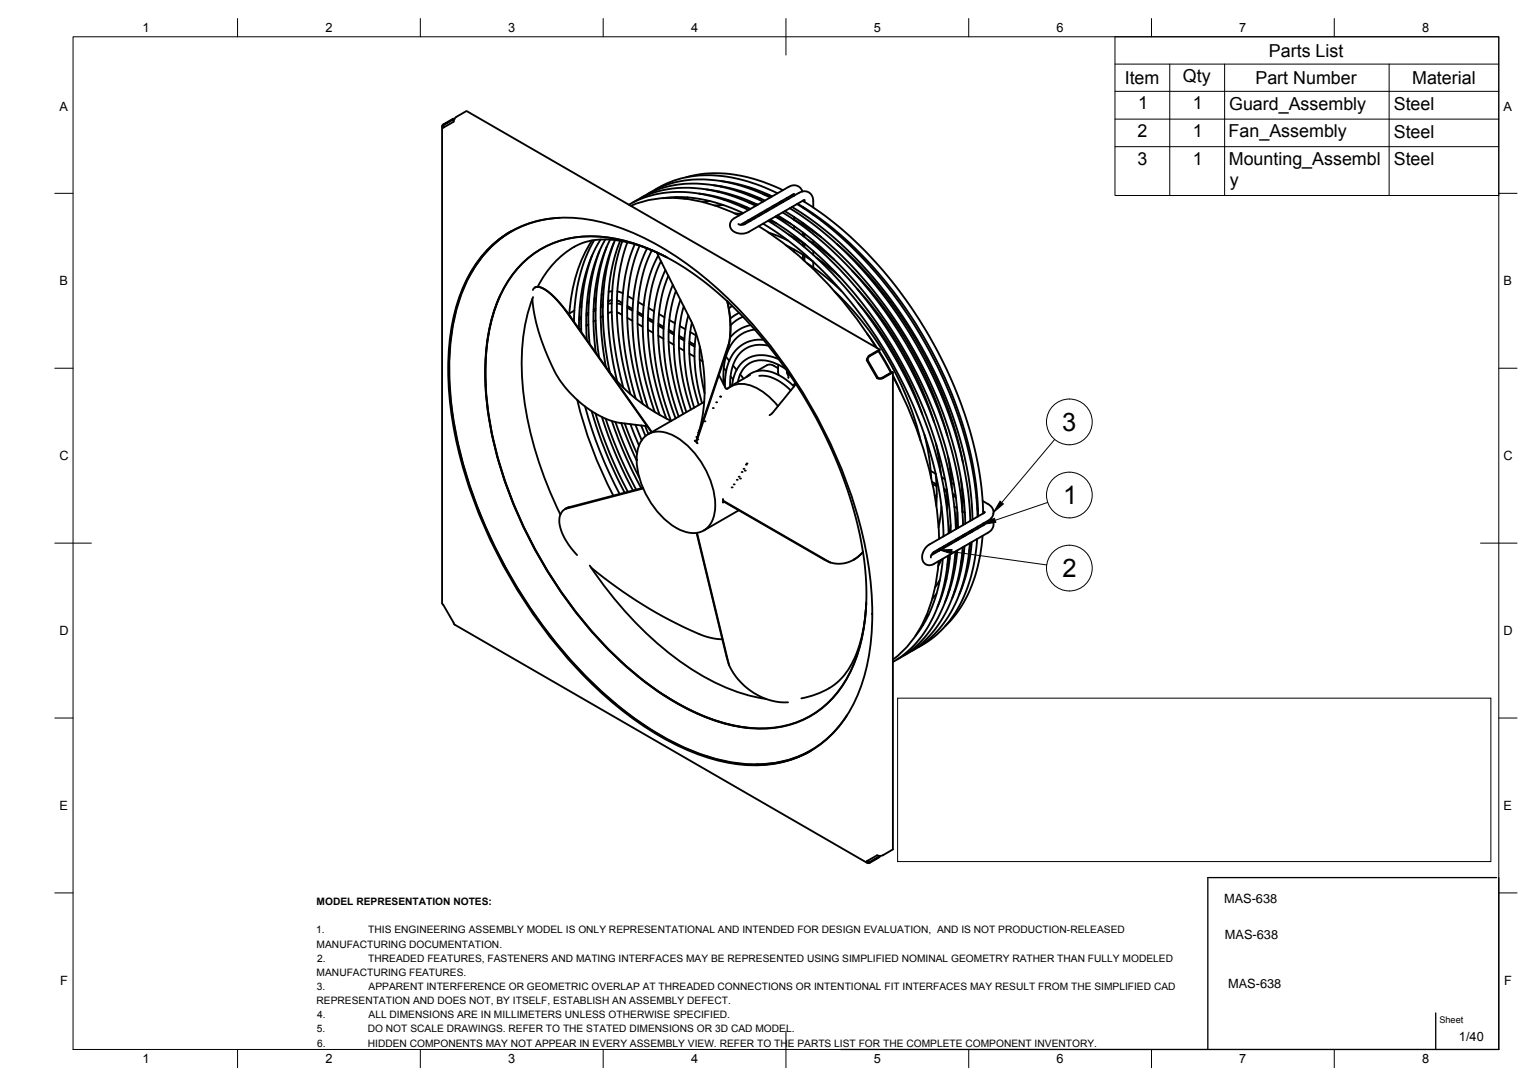
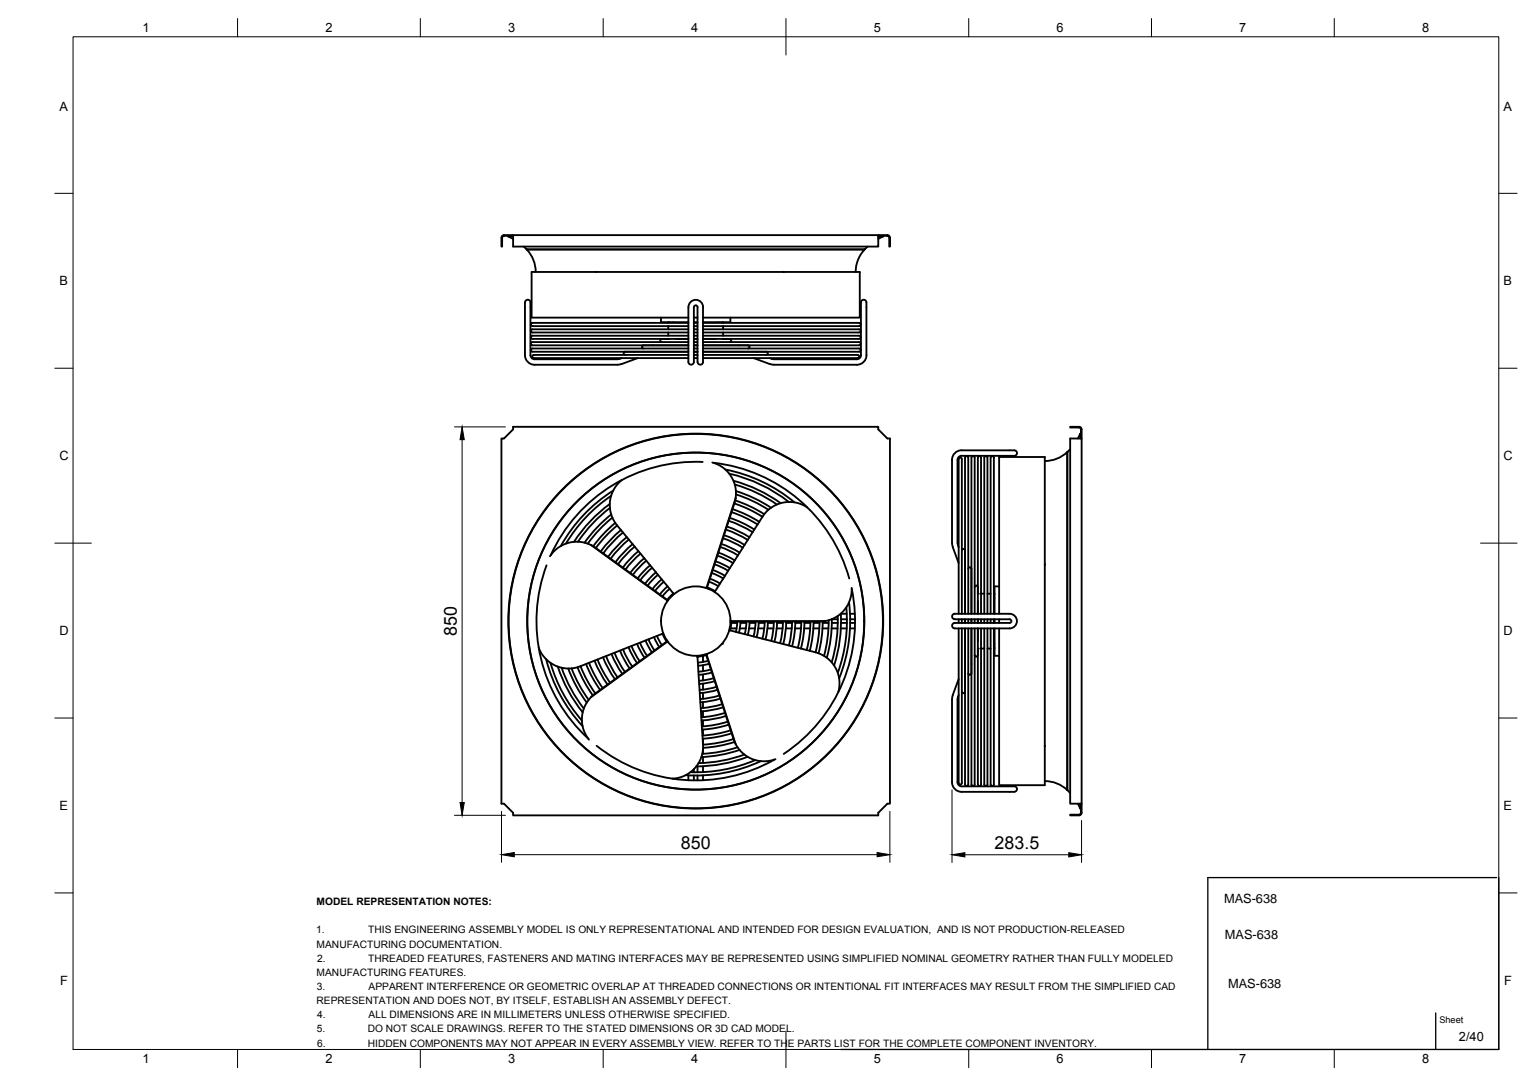
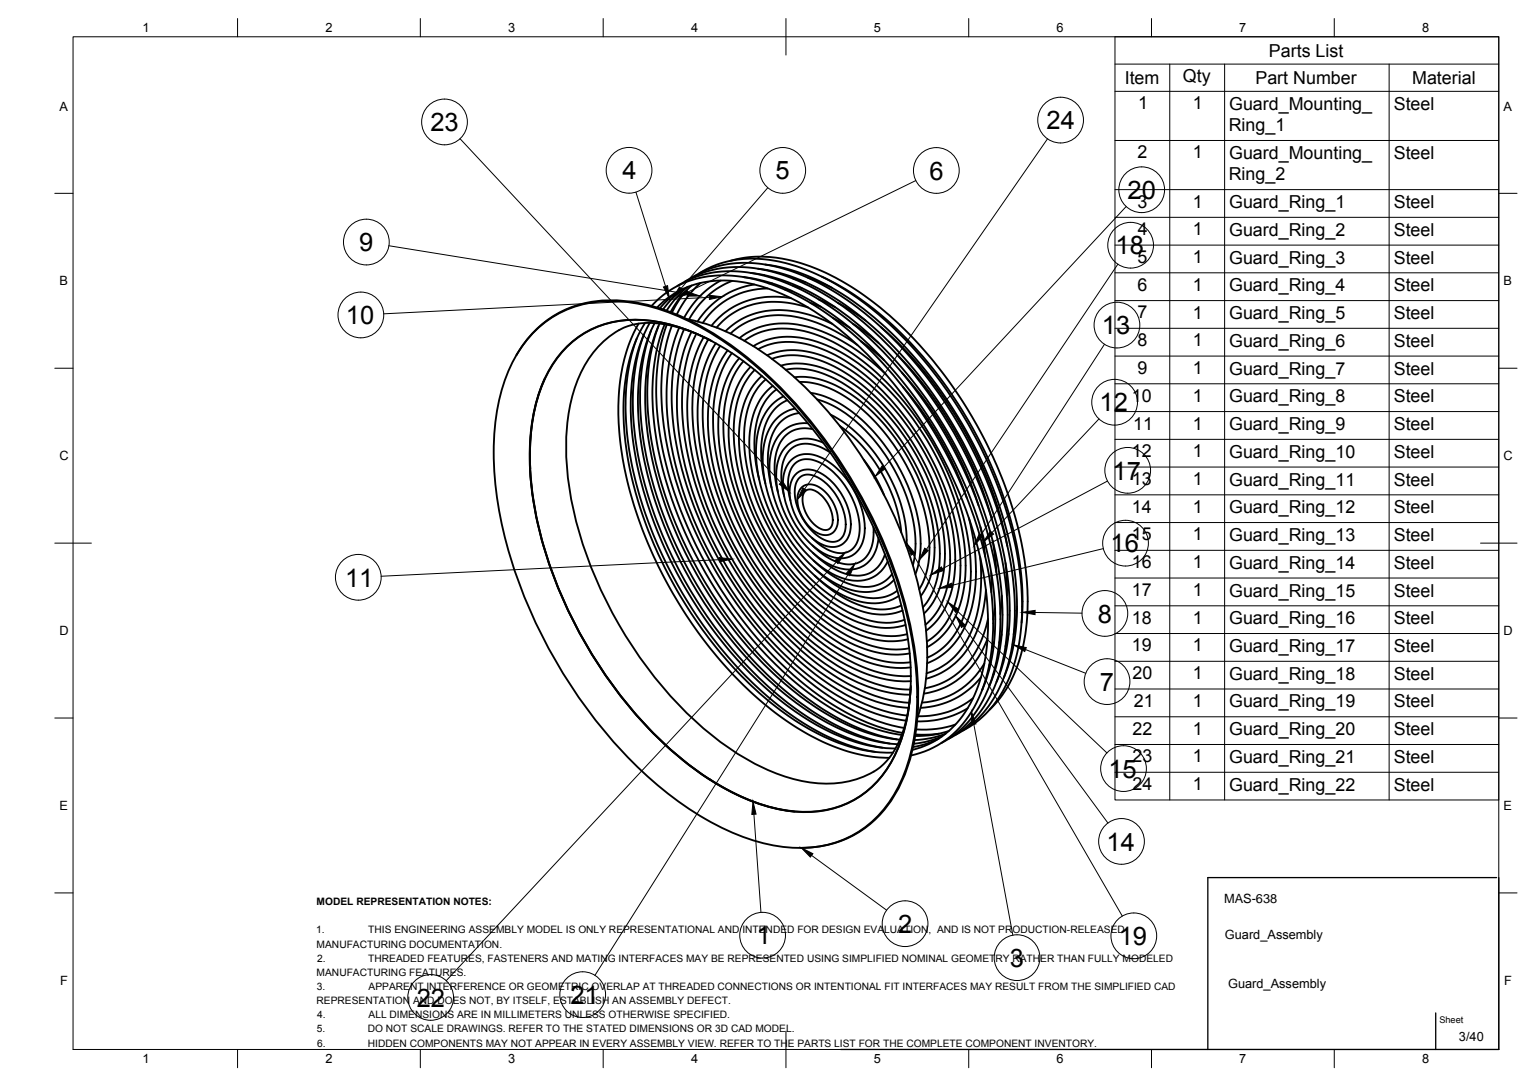
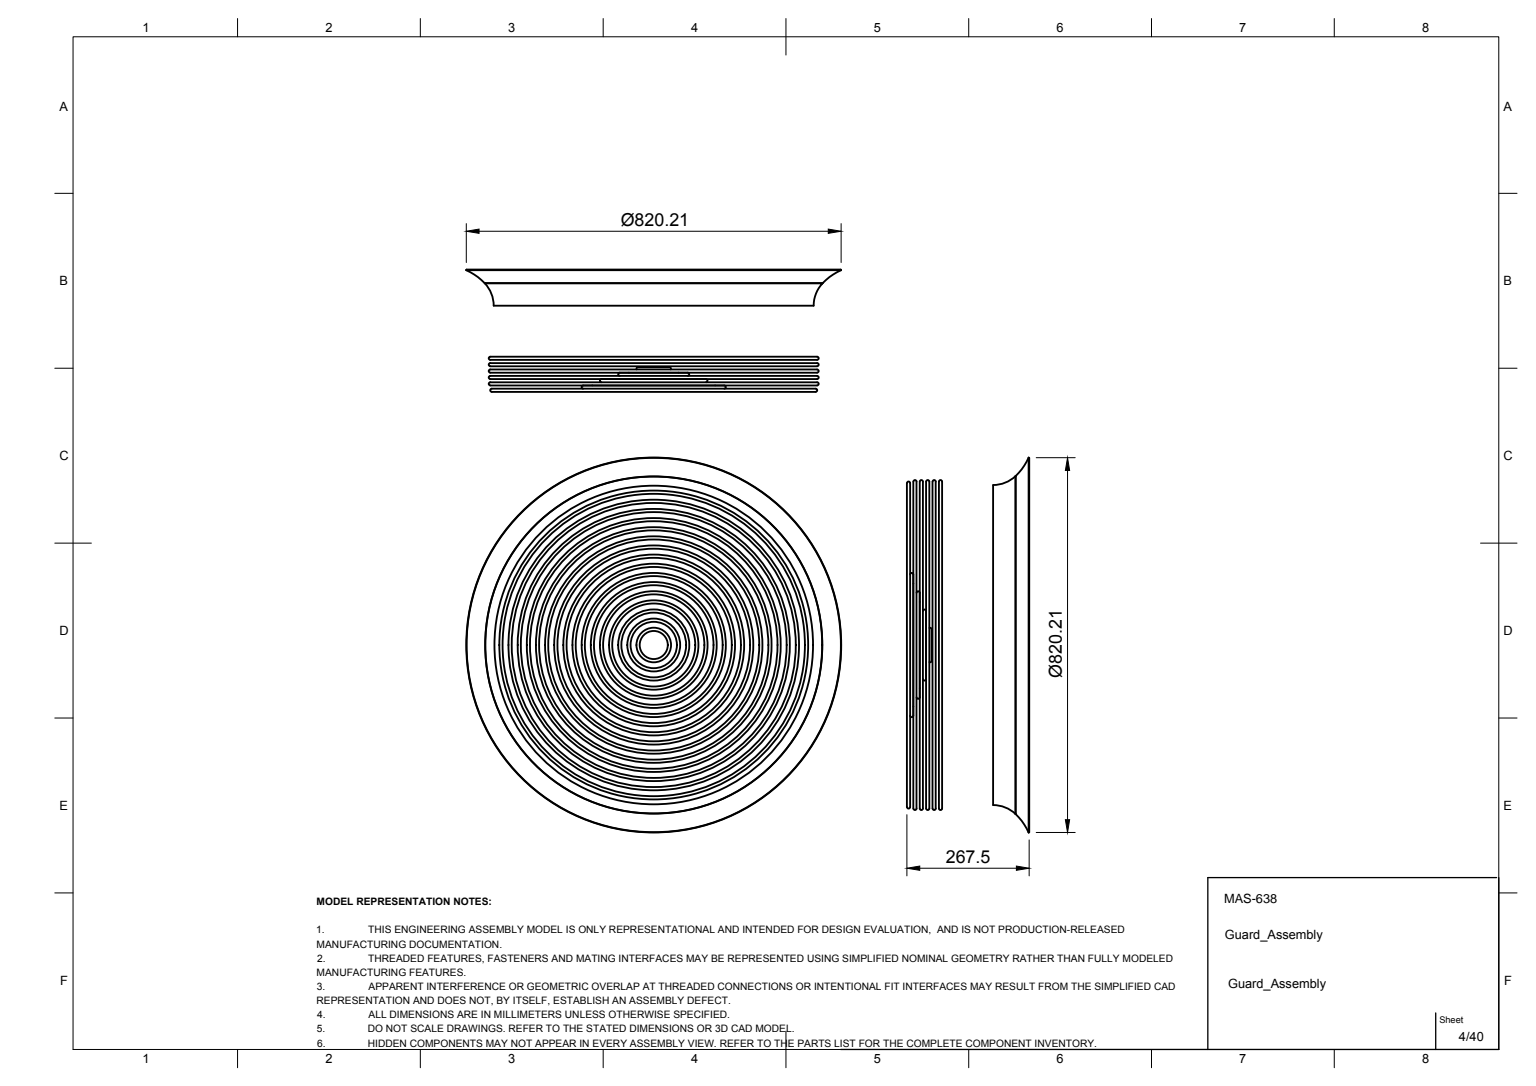
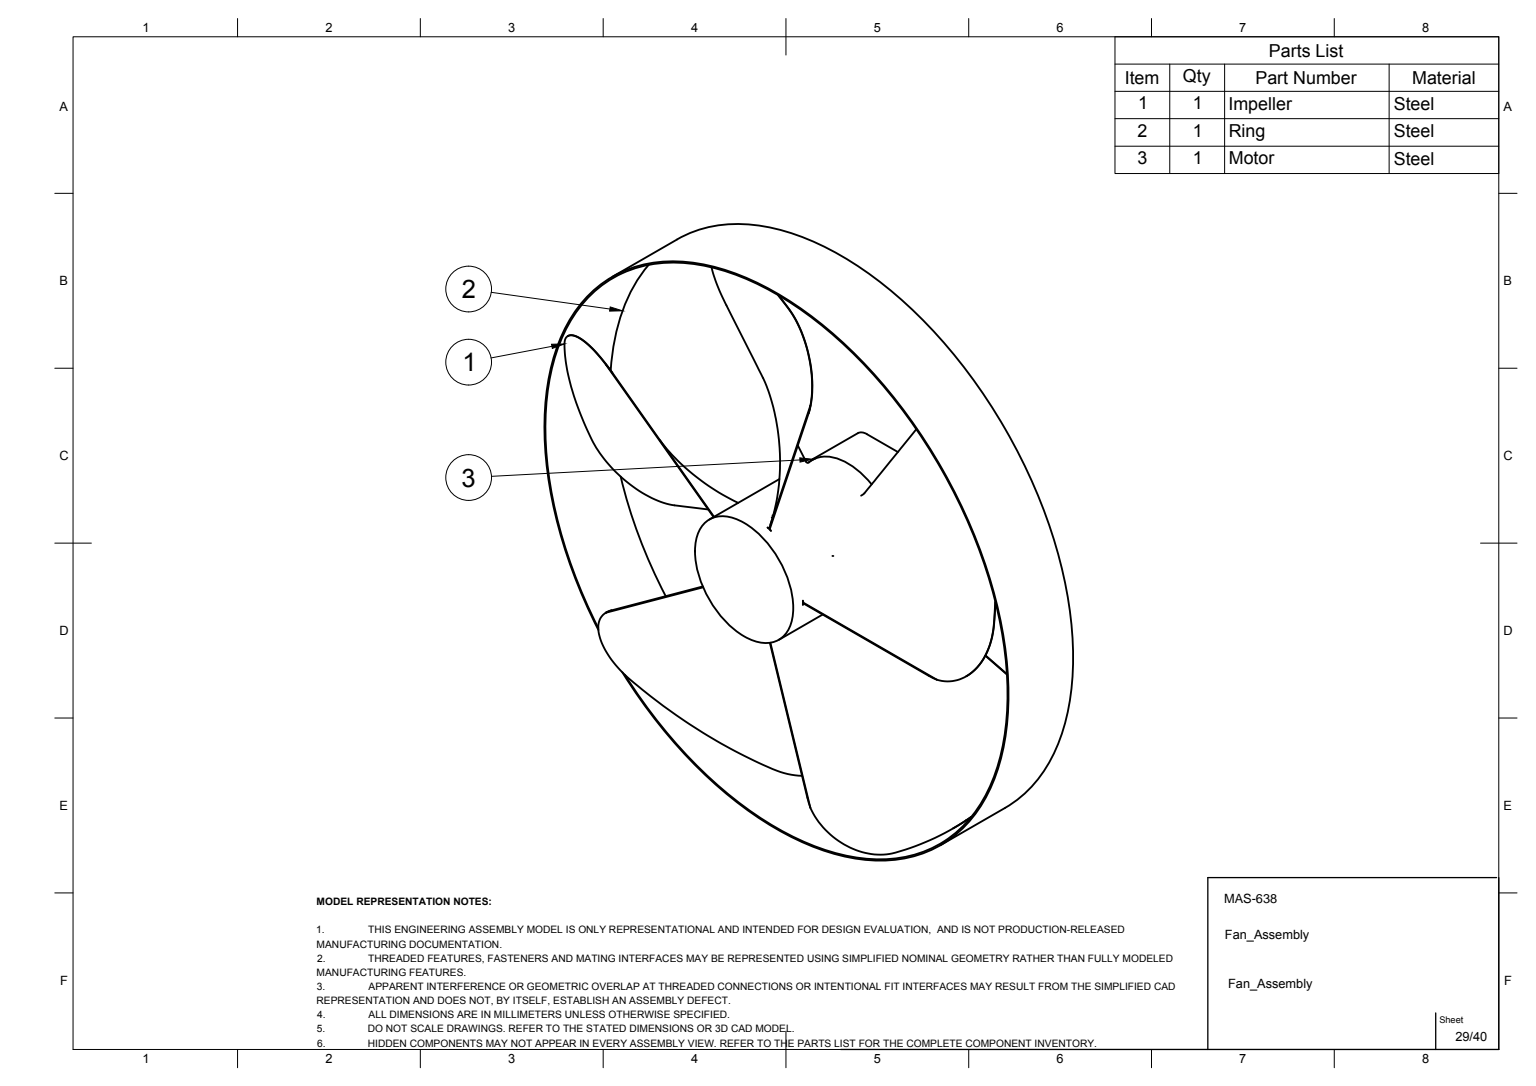
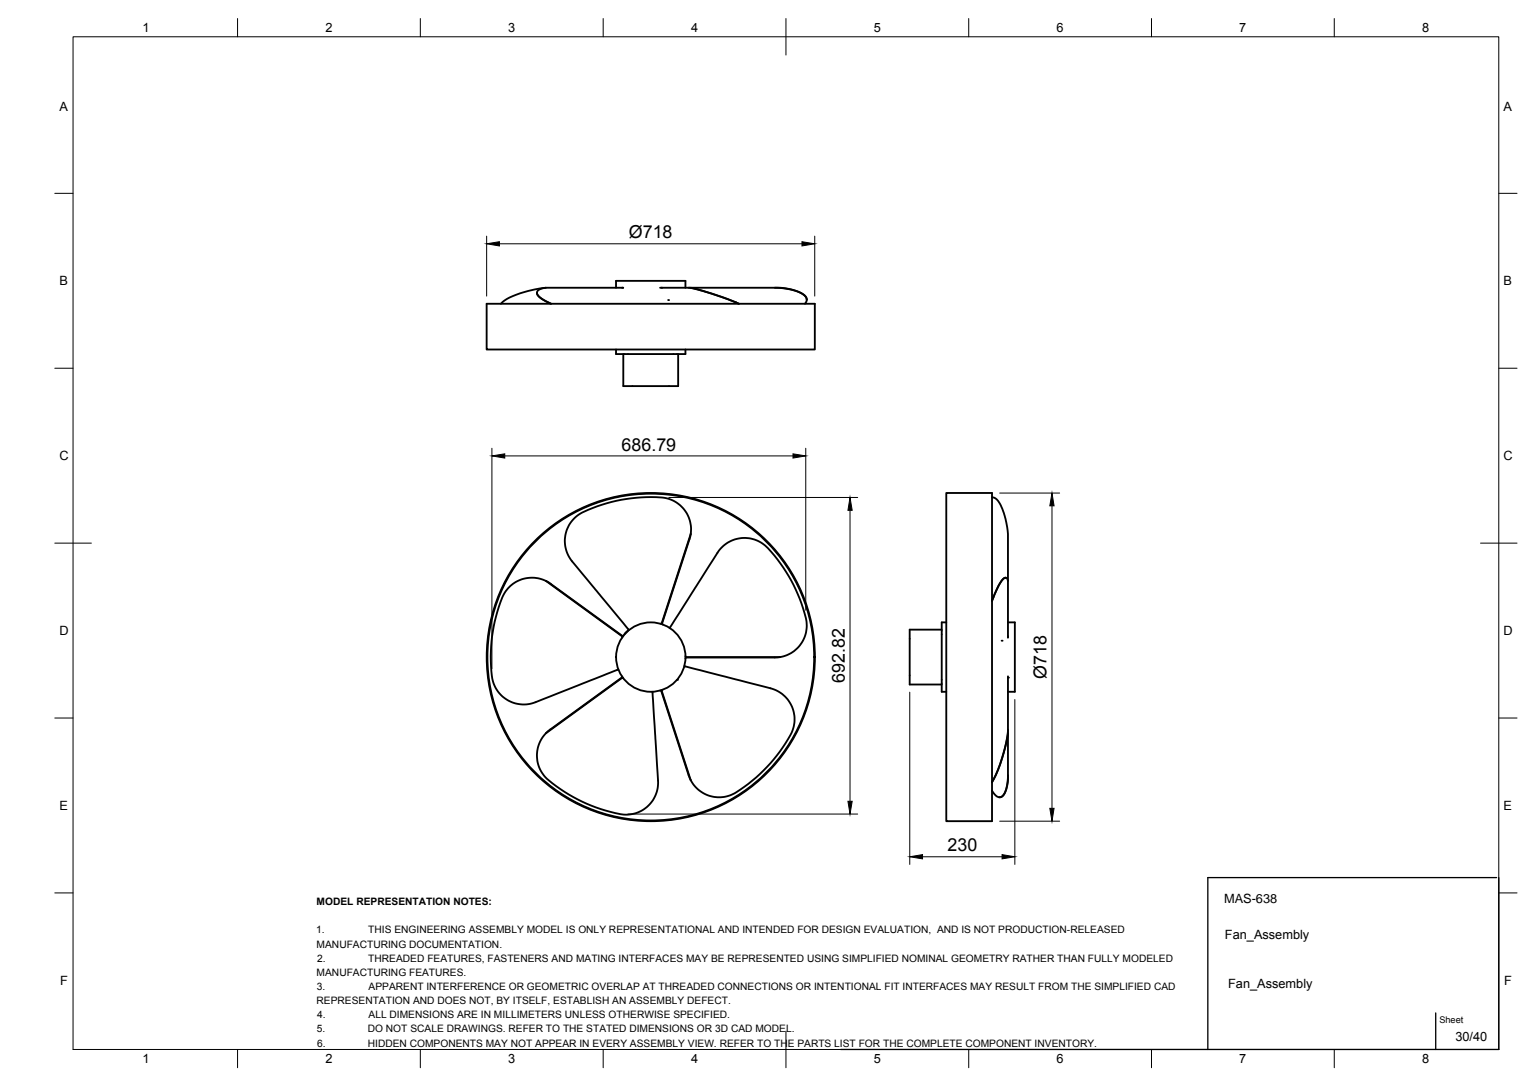
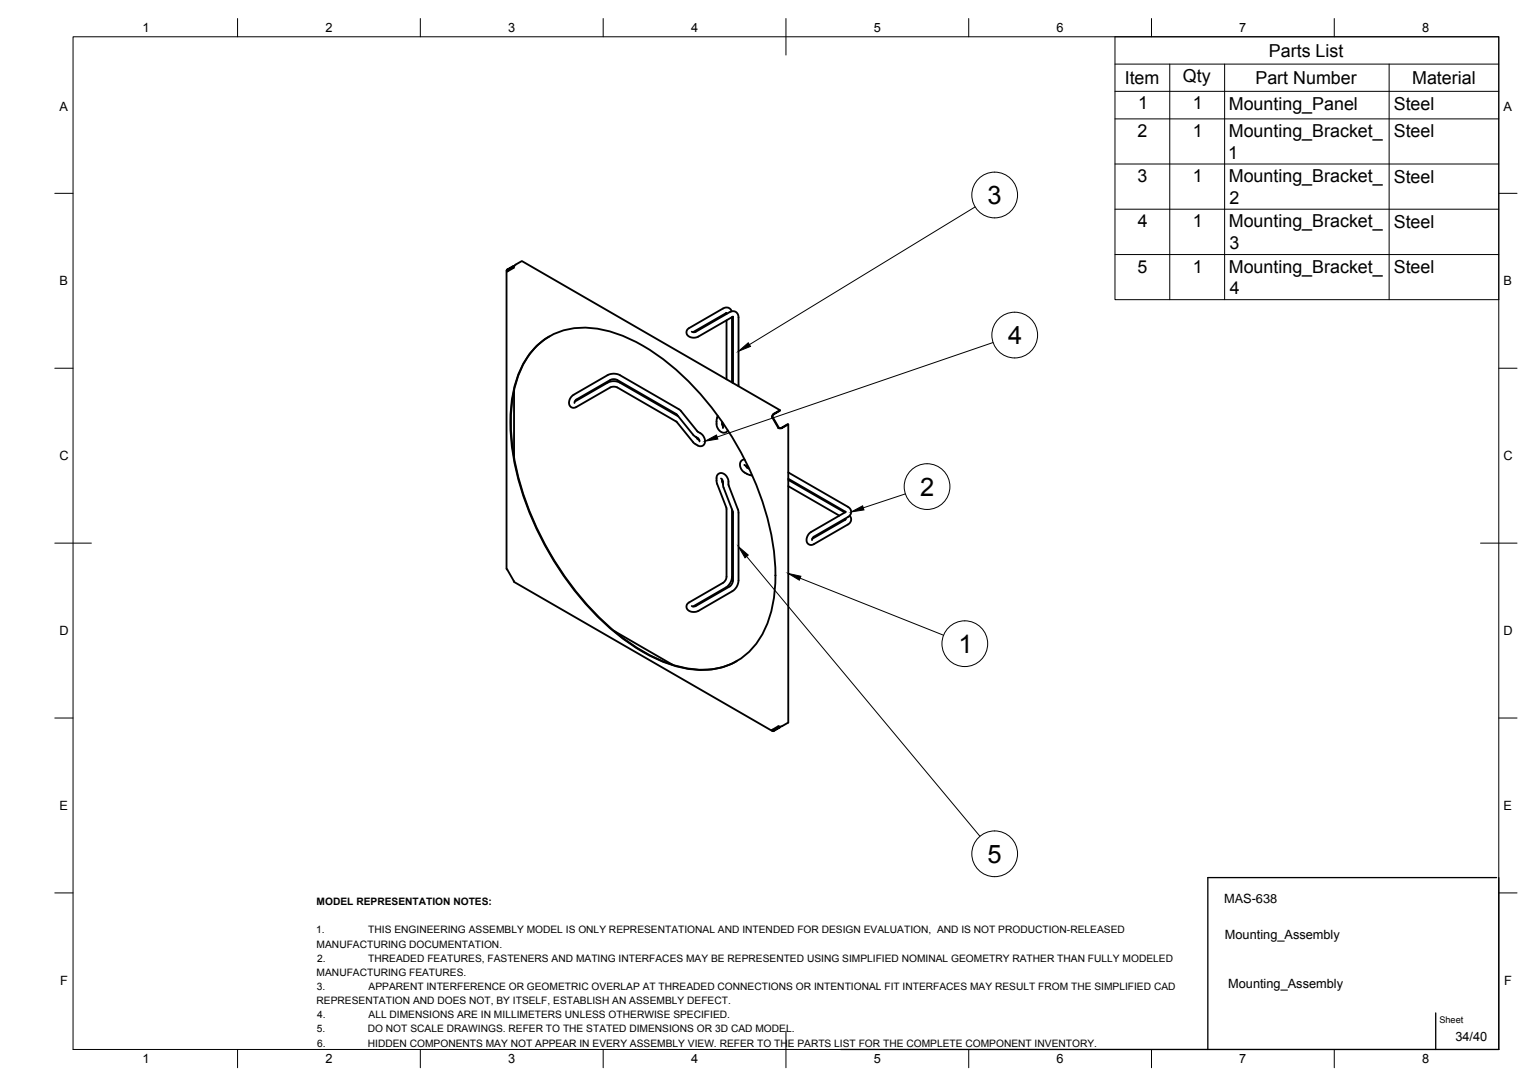
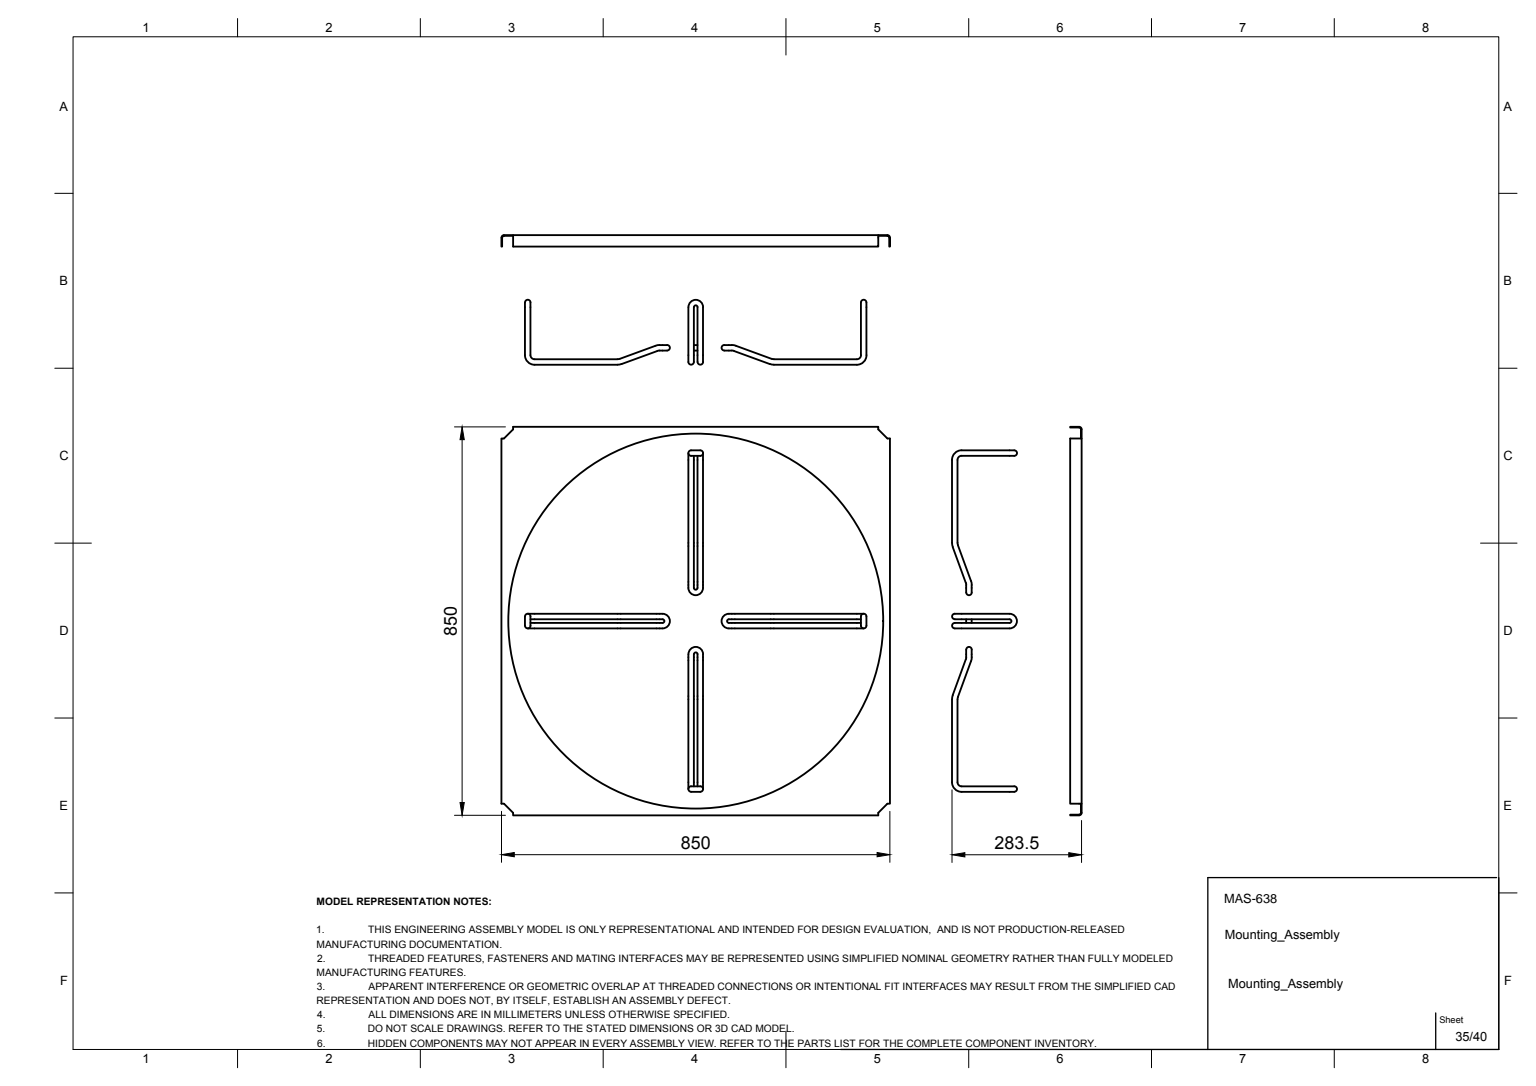
ISO-10303-21;
HEADER;
FILE_DESCRIPTION((''),'2;1');
FILE_NAME('MAS-638','2026-10-09T12:00:21-07:00',(''),(''),'','','');
FILE_SCHEMA (('AUTOMOTIVE_DESIGN { 1 0 10303 214 3 1 1 }'));
ENDSEC;
DATA;
#10 = MECHANICAL_DESIGN_GEOMETRIC_PRESENTATION_REPRESENTATION('',(#396,#397,
#398,#399,#400,#401,#402,#403,#404,#405,#406,#407,#408,#409,#410,#411,#412,
#413,#414,#415,#416,#417,#418,#419,#420,#421,#422,#423,#424,#425,#426,#427,
#428,#429,#430,#431,#432,#433,#434,#435),#10334) ;
#11 = (
BOUNDED_CURVE()
B_SPLINE_CURVE(2,(#6661,#6662,#6663,#6664,#6665,#6666,#6667,#6668,#6669,
#6670,#6671,#6672,#6673,#6674,#6675),.UNSPECIFIED.,.F.,.F.)
B_SPLINE_CURVE_WITH_KNOTS((3,2,2,2,2,2,2,3),(0.24767599272402,0.275737101138962,
0.367649468185283,0.459561835231604,0.551474202277924,0.643386569324245,
0.735298936370566,0.744991303101576),.UNSPECIFIED.)
CURVE()
GEOMETRIC_REPRESENTATION_ITEM()
RATIONAL_B_SPLINE_CURVE((0.999547382800022,0.999674234156792,1.,0.998932974802372,
1.,0.998932974802372,1.,0.998932974802372,1.,0.998932974802372,1.,0.998932974802372,
1.,0.999887479782547,0.999798690587312))
REPRESENTATION_ITEM('')
) ;
#12 = (
BOUNDED_CURVE()
B_SPLINE_CURVE(2,(#6842,#6843,#6844,#6845,#6846,#6847,#6848,#6849,#6850,
#6851,#6852,#6853,#6854,#6855,#6856),.UNSPECIFIED.,.F.,.F.)
B_SPLINE_CURVE_WITH_KNOTS((3,2,2,2,2,2,2,3),(0.0400825883740044,0.0441176470588235,
0.0588235294117647,0.0735294117647059,0.0882352941176471,0.102941176470588,
0.117647058823529,0.119652613204452),.UNSPECIFIED.)
CURVE()
GEOMETRIC_REPRESENTATION_ITEM()
RATIONAL_B_SPLINE_CURVE((0.999575116080077,0.999707225368239,1.,0.998932974802372,
1.,0.998932974802372,1.,0.998932974802372,1.,0.998932974802372,1.,0.998932974802372,
1.,0.999854481559943,0.999748654059601))
REPRESENTATION_ITEM('')
) ;
#13 = (
BOUNDED_CURVE()
B_SPLINE_CURVE(2,(#7299,#7300,#7301,#7302,#7303,#7304,#7305,#7306,#7307,
#7308,#7309,#7310,#7311,#7312,#7313),.UNSPECIFIED.,.F.,.F.)
B_SPLINE_CURVE_WITH_KNOTS((3,2,2,2,2,2,2,3),(0.24767599272402,0.275737101138962,
0.367649468185283,0.459561835231604,0.551474202277924,0.643386569324245,
0.735298936370566,0.744991303101576),.UNSPECIFIED.)
CURVE()
GEOMETRIC_REPRESENTATION_ITEM()
RATIONAL_B_SPLINE_CURVE((0.999547382800022,0.999674234156792,1.,0.998932974802372,
1.,0.998932974802372,1.,0.998932974802372,1.,0.998932974802372,1.,0.998932974802372,
1.,0.999887479782547,0.999798690587312))
REPRESENTATION_ITEM('')
) ;
#14 = (
BOUNDED_CURVE()
B_SPLINE_CURVE(2,(#7480,#7481,#7482,#7483,#7484,#7485,#7486,#7487,#7488,
#7489,#7490,#7491,#7492,#7493,#7494),.UNSPECIFIED.,.F.,.F.)
B_SPLINE_CURVE_WITH_KNOTS((3,2,2,2,2,2,2,3),(0.0400825883740044,0.0441176470588235,
0.0588235294117647,0.0735294117647059,0.0882352941176471,0.102941176470588,
0.117647058823529,0.119652613204452),.UNSPECIFIED.)
CURVE()
GEOMETRIC_REPRESENTATION_ITEM()
RATIONAL_B_SPLINE_CURVE((0.999575116080077,0.999707225368239,1.,0.998932974802372,
1.,0.998932974802372,1.,0.998932974802372,1.,0.998932974802372,1.,0.998932974802372,
1.,0.999854481559943,0.999748654059601))
REPRESENTATION_ITEM('')
) ;
#15 = (
BOUNDED_CURVE()
B_SPLINE_CURVE(2,(#7937,#7938,#7939,#7940,#7941,#7942,#7943,#7944,#7945,
#7946,#7947,#7948,#7949,#7950,#7951),.UNSPECIFIED.,.F.,.F.)
B_SPLINE_CURVE_WITH_KNOTS((3,2,2,2,2,2,2,3),(0.24767599272402,0.275737101138962,
0.367649468185283,0.459561835231604,0.551474202277924,0.643386569324245,
0.735298936370566,0.744991303101576),.UNSPECIFIED.)
CURVE()
GEOMETRIC_REPRESENTATION_ITEM()
RATIONAL_B_SPLINE_CURVE((0.999547382800022,0.999674234156792,1.,0.998932974802372,
1.,0.998932974802372,1.,0.998932974802372,1.,0.998932974802372,1.,0.998932974802372,
1.,0.999887479782547,0.999798690587312))
REPRESENTATION_ITEM('')
) ;
#16 = (
BOUNDED_CURVE()
B_SPLINE_CURVE(2,(#8118,#8119,#8120,#8121,#8122,#8123,#8124,#8125,#8126,
#8127,#8128,#8129,#8130,#8131,#8132),.UNSPECIFIED.,.F.,.F.)
B_SPLINE_CURVE_WITH_KNOTS((3,2,2,2,2,2,2,3),(0.0400825883740044,0.0441176470588235,
0.0588235294117647,0.0735294117647059,0.0882352941176471,0.102941176470588,
0.117647058823529,0.119652613204452),.UNSPECIFIED.)
CURVE()
GEOMETRIC_REPRESENTATION_ITEM()
RATIONAL_B_SPLINE_CURVE((0.999575116080077,0.999707225368239,1.,0.998932974802372,
1.,0.998932974802372,1.,0.998932974802372,1.,0.998932974802372,1.,0.998932974802372,
1.,0.999854481559943,0.999748654059601))
REPRESENTATION_ITEM('')
) ;
#17 = (
BOUNDED_CURVE()
B_SPLINE_CURVE(2,(#8574,#8575,#8576,#8577,#8578,#8579,#8580,#8581,#8582,
#8583,#8584,#8585,#8586,#8587,#8588),.UNSPECIFIED.,.F.,.F.)
B_SPLINE_CURVE_WITH_KNOTS((3,2,2,2,2,2,2,3),(0.24767599272402,0.275737101138962,
0.367649468185283,0.459561835231603,0.551474202277924,0.643386569324245,
0.735298936370566,0.744991303101576),.UNSPECIFIED.)
CURVE()
GEOMETRIC_REPRESENTATION_ITEM()
RATIONAL_B_SPLINE_CURVE((0.999547382800022,0.999674234156792,1.,0.998932974802372,
1.,0.998932974802372,1.,0.998932974802372,1.,0.998932974802372,1.,0.998932974802372,
1.,0.999887479782547,0.999798690587312))
REPRESENTATION_ITEM('')
) ;
#18 = (
BOUNDED_CURVE()
B_SPLINE_CURVE(2,(#8755,#8756,#8757,#8758,#8759,#8760,#8761,#8762,#8763,
#8764,#8765,#8766,#8767,#8768,#8769),.UNSPECIFIED.,.F.,.F.)
B_SPLINE_CURVE_WITH_KNOTS((3,2,2,2,2,2,2,3),(0.0400825883740044,0.0441176470588235,
0.0588235294117647,0.0735294117647059,0.0882352941176471,0.102941176470588,
0.117647058823529,0.119652613204452),.UNSPECIFIED.)
CURVE()
GEOMETRIC_REPRESENTATION_ITEM()
RATIONAL_B_SPLINE_CURVE((0.999575116080077,0.999707225368239,1.,0.998932974802372,
1.,0.998932974802372,1.,0.998932974802372,1.,0.998932974802372,1.,0.998932974802372,
1.,0.999854481559943,0.999748654059601))
REPRESENTATION_ITEM('')
) ;
#19 = (
BOUNDED_CURVE()
B_SPLINE_CURVE(2,(#9211,#9212,#9213,#9214,#9215,#9216,#9217,#9218,#9219,
#9220,#9221,#9222,#9223,#9224,#9225),.UNSPECIFIED.,.F.,.F.)
B_SPLINE_CURVE_WITH_KNOTS((3,2,2,2,2,2,2,3),(0.24767599272402,0.275737101138962,
0.367649468185283,0.459561835231604,0.551474202277924,0.643386569324245,
0.735298936370566,0.744991303101576),.UNSPECIFIED.)
CURVE()
GEOMETRIC_REPRESENTATION_ITEM()
RATIONAL_B_SPLINE_CURVE((0.999547382800022,0.999674234156792,1.,0.998932974802372,
1.,0.998932974802372,1.,0.998932974802372,1.,0.998932974802372,1.,0.998932974802372,
1.,0.999887479782547,0.999798690587312))
REPRESENTATION_ITEM('')
) ;
#20 = (
BOUNDED_CURVE()
B_SPLINE_CURVE(2,(#9392,#9393,#9394,#9395,#9396,#9397,#9398,#9399,#9400,
#9401,#9402,#9403,#9404,#9405,#9406),.UNSPECIFIED.,.F.,.F.)
B_SPLINE_CURVE_WITH_KNOTS((3,2,2,2,2,2,2,3),(0.0400825883740044,0.0441176470588235,
0.0588235294117647,0.0735294117647059,0.0882352941176471,0.102941176470588,
0.117647058823529,0.119652613204452),.UNSPECIFIED.)
CURVE()
GEOMETRIC_REPRESENTATION_ITEM()
RATIONAL_B_SPLINE_CURVE((0.999575116080077,0.999707225368239,1.,0.998932974802372,
1.,0.998932974802372,1.,0.998932974802372,1.,0.998932974802372,1.,0.998932974802372,
1.,0.999854481559943,0.999748654059601))
REPRESENTATION_ITEM('')
) ;
#21 = ELLIPSE('',#4098,37.7772650531372,35.8772408571367) ;
#22 = ELLIPSE('',#4099,37.8497403828003,36.0198777791808) ;
#23 = ELLIPSE('',#4107,36.8921420435166,34.215760038751) ;
#24 = ELLIPSE('',#4108,36.1551251123153,32.8675469297647) ;
#25 = ELLIPSE('',#4116,37.0958421669686,34.5946418749128) ;
#26 = ELLIPSE('',#4117,37.8806839269163,36.0787426019938) ;
#27 = ELLIPSE('',#4124,37.6579384286729,35.6509558139733) ;
#28 = ELLIPSE('',#4125,37.3365253827658,35.0500856310496) ;
#29 = ELLIPSE('',#4132,38.4895046711754,37.2427567220046) ;
#30 = ELLIPSE('',#4133,37.7160972861981,35.7660825268951) ;
#31 = (
BOUNDED_SURFACE()
B_SPLINE_SURFACE(1,2,((#6503,#6504,#6505,#6506,#6507,#6508,#6509,#6510,
#6511,#6512,#6513,#6514,#6515,#6516,#6517,#6518,#6519,#6520,#6521,#6522,
#6523,#6524,#6525),(#6526,#6527,#6528,#6529,#6530,#6531,#6532,#6533,#6534,
#6535,#6536,#6537,#6538,#6539,#6540,#6541,#6542,#6543,#6544,#6545,#6546,
#6547,#6548)),.UNSPECIFIED.,.F.,.F.,.F.)
B_SPLINE_SURFACE_WITH_KNOTS((2,2),(3,2,2,2,2,2,2,2,2,2,2,3),(0.,1.),(-1.033109709591E-7,
0.0147058823529412,0.0294117647058824,0.0441176470588235,0.0588235294117647,
0.0735294117647059,0.0882352941176471,0.102941176470588,0.117647058823529,
0.132352941176471,0.147058823529412,0.159998951452637),.UNSPECIFIED.)
GEOMETRIC_REPRESENTATION_ITEM()
RATIONAL_B_SPLINE_SURFACE(((1.00000001499212,0.998932967306364,1.,0.998932974802372,
1.,0.998932974802372,1.,0.998932974802372,1.,0.998932974802372,1.,0.998932974802372,
1.,0.998932974802372,1.,0.998932974802372,1.,0.998932974802372,1.,0.998932974802372,
1.,0.999061093906287,0.999774528647208),(1.00000001499212,0.998932967306364,
1.,0.998932974802372,1.,0.998932974802372,1.,0.998932974802372,1.,0.998932974802372,
1.,0.998932974802372,1.,0.998932974802372,1.,0.998932974802372,1.,0.998932974802372,
1.,0.998932974802372,1.,0.999061093906287,0.999774528647208)))
REPRESENTATION_ITEM('')
SURFACE()
) ;
#32 = (
BOUNDED_SURFACE()
B_SPLINE_SURFACE(1,2,((#6692,#6693,#6694,#6695,#6696,#6697,#6698,#6699,
#6700,#6701,#6702,#6703,#6704,#6705,#6706,#6707,#6708,#6709,#6710,#6711,
#6712,#6713,#6714),(#6715,#6716,#6717,#6718,#6719,#6720,#6721,#6722,#6723,
#6724,#6725,#6726,#6727,#6728,#6729,#6730,#6731,#6732,#6733,#6734,#6735,
#6736,#6737)),.UNSPECIFIED.,.F.,.F.,.F.)
B_SPLINE_SURFACE_WITH_KNOTS((2,2),(3,2,2,2,2,2,2,2,2,2,2,3),(-2.12079707674176E-9,
1.),(-4.92610673029739E-10,0.0147058823529412,0.0294117647058824,0.0441176470588235,
0.0588235294117647,0.0735294117647059,0.0882352941176471,0.102941176470588,
0.117647058823529,0.132352941176471,0.147058823529412,0.159999479208712),
 .UNSPECIFIED.)
GEOMETRIC_REPRESENTATION_ITEM()
RATIONAL_B_SPLINE_SURFACE(((1.00000000007149,0.99893297476663,1.,0.998932974802372,
1.,0.998932974802372,1.,0.998932974802372,1.,0.998932974802372,1.,0.998932974802372,
1.,0.998932974802372,1.,0.998932974802372,1.,0.998932974802372,1.,0.998932974802372,
1.,0.999061055613513,0.999774586844051),(1.00000000007149,0.99893297476663,
1.,0.998932974802372,1.,0.998932974802372,1.,0.998932974802372,1.,0.998932974802372,
1.,0.998932974802372,1.,0.998932974802372,1.,0.998932974802372,1.,0.998932974802372,
1.,0.998932974802372,1.,0.999061055613513,0.999774586844051)))
REPRESENTATION_ITEM('')
SURFACE()
) ;
#33 = (
BOUNDED_SURFACE()
B_SPLINE_SURFACE(3,2,((#6905,#6906,#6907),(#6908,#6909,#6910),(#6911,#6912,
#6913),(#6914,#6915,#6916),(#6917,#6918,#6919),(#6920,#6921,#6922),(#6923,
#6924,#6925),(#6926,#6927,#6928),(#6929,#6930,#6931),(#6932,#6933,#6934),
(#6935,#6936,#6937),(#6938,#6939,#6940),(#6941,#6942,#6943),(#6944,#6945,
#6946),(#6947,#6948,#6949),(#6950,#6951,#6952),(#6953,#6954,#6955),(#6956,
#6957,#6958),(#6959,#6960,#6961),(#6962,#6963,#6964),(#6965,#6966,#6967),
(#6968,#6969,#6970),(#6971,#6972,#6973),(#6974,#6975,#6976),(#6977,#6978,
#6979),(#6980,#6981,#6982),(#6983,#6984,#6985),(#6986,#6987,#6988),(#6989,
#6990,#6991),(#6992,#6993,#6994),(#6995,#6996,#6997),(#6998,#6999,#7000)),
 .UNSPECIFIED.,.F.,.F.,.F.)
B_SPLINE_SURFACE_WITH_KNOTS((4,2,2,2,2,2,2,2,2,2,2,2,2,2,2,4),(3,3),(0.0363322941033848,
0.0552795959345893,0.0647532468501916,0.0742268977657938,0.0837005486813961,
0.0931741995969984,0.102647850512601,0.112121501428203,0.121595152343805,
0.131068803259407,0.14054245417501,0.150016105090612,0.159489756006214,
0.168963406921816,0.178437057837419,0.187910708753021),(0.,1.),
 .UNSPECIFIED.)
GEOMETRIC_REPRESENTATION_ITEM()
RATIONAL_B_SPLINE_SURFACE(((1.,0.713723577868364,1.),(1.,0.713722445293404,
1.),(1.,0.713725662281373,1.),(1.,0.713724573699931,1.),(1.,0.71372208949302,
1.),(1.,0.713725723145716,1.),(1.,0.713725237219869,1.),(1.,0.713719633392001,
1.),(1.,0.713725477091233,1.),(1.,0.713724228403321,1.),(1.,0.713722641415878,
1.),(1.,0.713725747691194,1.),(1.,0.713724999814938,1.),(1.,0.713718882742839,
1.),(1.,0.713725607158444,1.),(1.,0.713723850204247,1.),(1.,0.713723140250565,
1.),(1.,0.713725729945787,1.),(1.,0.713724718679381,1.),(1.,0.713718072353828,
1.),(1.,0.713725695695606,1.),(1.,0.713723420086558,1.),(1.,0.713723588770072,
1.),(1.,0.71372566780113,1.),(1.,0.713718399163855,1.),(1.,0.713724843902384,
1.),(1.,0.713725741663279,1.),(1.,0.71372293985685,1.),(1.,0.713724004994082,
1.),(1.,0.713725560151496,1.),(1.,0.713723126093937,1.),(1.,0.713721352883454,
1.)))
REPRESENTATION_ITEM('')
SURFACE()
) ;
#34 = (
BOUNDED_SURFACE()
B_SPLINE_SURFACE(3,2,((#7001,#7002,#7003),(#7004,#7005,#7006),(#7007,#7008,
#7009),(#7010,#7011,#7012),(#7013,#7014,#7015),(#7016,#7017,#7018),(#7019,
#7020,#7021),(#7022,#7023,#7024),(#7025,#7026,#7027),(#7028,#7029,#7030),
(#7031,#7032,#7033),(#7034,#7035,#7036),(#7037,#7038,#7039),(#7040,#7041,
#7042),(#7043,#7044,#7045),(#7046,#7047,#7048),(#7049,#7050,#7051),(#7052,
#7053,#7054),(#7055,#7056,#7057),(#7058,#7059,#7060),(#7061,#7062,#7063),
(#7064,#7065,#7066),(#7067,#7068,#7069),(#7070,#7071,#7072),(#7073,#7074,
#7075),(#7076,#7077,#7078),(#7079,#7080,#7081),(#7082,#7083,#7084),(#7085,
#7086,#7087),(#7088,#7089,#7090),(#7091,#7092,#7093),(#7094,#7095,#7096),
(#7097,#7098,#7099),(#7100,#7101,#7102),(#7103,#7104,#7105),(#7106,#7107,
#7108)),.UNSPECIFIED.,.F.,.F.,.F.)
B_SPLINE_SURFACE_WITH_KNOTS((4,2,2,2,2,2,2,2,2,2,2,2,2,2,2,2,2,4),(3,3),
(0.110192674671804,0.119968567976379,0.129744461280954,0.139520354585529,
0.149296247890104,0.159072141194679,0.168848034499254,0.178623927803829,
0.183511874456117,0.188399821108404,0.198175714412979,0.207951607717554,
0.217727501022129,0.227503394326704,0.23727928763128,0.247055180935855,
0.25683107424043,0.266606967545005),(0.,1.),.UNSPECIFIED.)
GEOMETRIC_REPRESENTATION_ITEM()
RATIONAL_B_SPLINE_SURFACE(((1.,0.717557917014249,1.),(1.,0.717557424551413,
1.),(1.,0.717562701205404,1.),(1.,0.717561702803317,1.),(1.,0.717559005659748,
1.),(1.,0.717563327413176,1.),(1.,0.71756229100789,1.),(1.,0.717553816681041,
1.),(1.,0.717563248342644,1.),(1.,0.717560128438615,1.),(1.,0.717560865936392,
1.),(1.,0.717563079897794,1.),(1.,0.717555152418623,1.),(1.,0.717562714682237,
1.),(1.,0.717563278057682,1.),(1.,0.717559267705998,1.),(1.,0.717558273919951,
1.),(1.,0.717561484503512,1.),(1.,0.717562276054518,1.),(1.,0.717562227727252,
1.),(1.,0.717558058641825,1.),(1.,0.717563288924202,1.),(1.,0.717562675856868,
1.),(1.,0.717554973696268,1.),(1.,0.717563128955385,1.),(1.,0.717560719068534,
1.),(1.,0.717560347129028,1.),(1.,0.717563217875631,1.),(1.,0.717554301335648,
1.),(1.,0.717562479166741,1.),(1.,0.717563325990987,1.),(1.,0.717558566722815,
1.),(1.,0.717561980919154,1.),(1.,0.717562507369476,1.),(1.,0.717555378743213,
1.),(1.,0.717566078456111,1.)))
REPRESENTATION_ITEM('')
SURFACE()
) ;
#35 = (
BOUNDED_SURFACE()
B_SPLINE_SURFACE(1,2,((#7141,#7142,#7143,#7144,#7145,#7146,#7147,#7148,
#7149,#7150,#7151,#7152,#7153,#7154,#7155,#7156,#7157,#7158,#7159,#7160,
#7161,#7162,#7163),(#7164,#7165,#7166,#7167,#7168,#7169,#7170,#7171,#7172,
#7173,#7174,#7175,#7176,#7177,#7178,#7179,#7180,#7181,#7182,#7183,#7184,
#7185,#7186)),.UNSPECIFIED.,.F.,.F.,.F.)
B_SPLINE_SURFACE_WITH_KNOTS((2,2),(3,2,2,2,2,2,2,2,2,2,2,3),(0.,1.),(-1.03310890689824E-7,
0.0147058823529412,0.0294117647058824,0.0441176470588235,0.0588235294117647,
0.0735294117647059,0.0882352941176471,0.102941176470588,0.117647058823529,
0.132352941176471,0.147058823529412,0.159998951452637),.UNSPECIFIED.)
GEOMETRIC_REPRESENTATION_ITEM()
RATIONAL_B_SPLINE_SURFACE(((1.00000001499211,0.99893296730637,1.,0.998932974802372,
1.,0.998932974802372,1.,0.998932974802372,1.,0.998932974802372,1.,0.998932974802372,
1.,0.998932974802372,1.,0.998932974802372,1.,0.998932974802372,1.,0.998932974802372,
1.,0.999061093906287,0.999774528647208),(1.00000001499211,0.99893296730637,
1.,0.998932974802372,1.,0.998932974802372,1.,0.998932974802372,1.,0.998932974802372,
1.,0.998932974802372,1.,0.998932974802372,1.,0.998932974802372,1.,0.998932974802372,
1.,0.998932974802372,1.,0.999061093906287,0.999774528647208)))
REPRESENTATION_ITEM('')
SURFACE()
) ;
#36 = (
BOUNDED_SURFACE()
B_SPLINE_SURFACE(1,2,((#7330,#7331,#7332,#7333,#7334,#7335,#7336,#7337,
#7338,#7339,#7340,#7341,#7342,#7343,#7344,#7345,#7346,#7347,#7348,#7349,
#7350,#7351,#7352),(#7353,#7354,#7355,#7356,#7357,#7358,#7359,#7360,#7361,
#7362,#7363,#7364,#7365,#7366,#7367,#7368,#7369,#7370,#7371,#7372,#7373,
#7374,#7375)),.UNSPECIFIED.,.F.,.F.,.F.)
B_SPLINE_SURFACE_WITH_KNOTS((2,2),(3,2,2,2,2,2,2,2,2,2,2,3),(-2.12079713977352E-9,
1.),(-4.92610737156842E-10,0.0147058823529412,0.0294117647058824,0.0441176470588235,
0.0588235294117647,0.0735294117647059,0.0882352941176471,0.102941176470588,
0.117647058823529,0.132352941176471,0.147058823529412,0.159999479208712),
 .UNSPECIFIED.)
GEOMETRIC_REPRESENTATION_ITEM()
RATIONAL_B_SPLINE_SURFACE(((1.00000000007149,0.99893297476663,1.,0.998932974802372,
1.,0.998932974802372,1.,0.998932974802372,1.,0.998932974802372,1.,0.998932974802372,
1.,0.998932974802372,1.,0.998932974802372,1.,0.998932974802372,1.,0.998932974802372,
1.,0.999061055613513,0.999774586844051),(1.00000000007149,0.99893297476663,
1.,0.998932974802372,1.,0.998932974802372,1.,0.998932974802372,1.,0.998932974802372,
1.,0.998932974802372,1.,0.998932974802372,1.,0.998932974802372,1.,0.998932974802372,
1.,0.998932974802372,1.,0.999061055613513,0.999774586844051)))
REPRESENTATION_ITEM('')
SURFACE()
) ;
#37 = (
BOUNDED_SURFACE()
B_SPLINE_SURFACE(3,2,((#7542,#7543,#7544),(#7545,#7546,#7547),(#7548,#7549,
#7550),(#7551,#7552,#7553),(#7554,#7555,#7556),(#7557,#7558,#7559),(#7560,
#7561,#7562),(#7563,#7564,#7565),(#7566,#7567,#7568),(#7569,#7570,#7571),
(#7572,#7573,#7574),(#7575,#7576,#7577),(#7578,#7579,#7580),(#7581,#7582,
#7583),(#7584,#7585,#7586),(#7587,#7588,#7589),(#7590,#7591,#7592),(#7593,
#7594,#7595),(#7596,#7597,#7598),(#7599,#7600,#7601),(#7602,#7603,#7604),
(#7605,#7606,#7607),(#7608,#7609,#7610),(#7611,#7612,#7613),(#7614,#7615,
#7616),(#7617,#7618,#7619),(#7620,#7621,#7622),(#7623,#7624,#7625),(#7626,
#7627,#7628),(#7629,#7630,#7631),(#7632,#7633,#7634),(#7635,#7636,#7637)),
 .UNSPECIFIED.,.F.,.F.,.F.)
B_SPLINE_SURFACE_WITH_KNOTS((4,2,2,2,2,2,2,2,2,2,2,2,2,2,2,4),(3,3),(0.0363322941033848,
0.0552795959345893,0.0647532468501916,0.0742268977657939,0.0837005486813961,
0.0931741995969984,0.102647850512601,0.112121501428203,0.121595152343805,
0.131068803259407,0.14054245417501,0.150016105090612,0.159489756006214,
0.168963406921816,0.178437057837419,0.187910708753021),(0.,1.),
 .UNSPECIFIED.)
GEOMETRIC_REPRESENTATION_ITEM()
RATIONAL_B_SPLINE_SURFACE(((1.,0.713723577868379,1.),(1.,0.71372244527551,
1.),(1.,0.713725662305176,1.),(1.,0.713724573687971,1.),(1.,0.713722089554594,
1.),(1.,0.713725723084203,1.),(1.,0.713725237316385,1.),(1.,0.71371963329541,
1.),(1.,0.713725477094868,1.),(1.,0.713724228399586,1.),(1.,0.713722641372577,
1.),(1.,0.713725747734493,1.),(1.,0.713724999822108,1.),(1.,0.713718882735633,
1.),(1.,0.713725607168583,1.),(1.,0.713723850194029,1.),(1.,0.713723140179135,
1.),(1.,0.713725730017236,1.),(1.,0.713724718641669,1.),(1.,0.713718072391505,
1.),(1.,0.713725695688412,1.),(1.,0.713723420093739,1.),(1.,0.713723588714817,
1.),(1.,0.71372566785642,1.),(1.,0.713718399180568,1.),(1.,0.713724843885739,
1.),(1.,0.713725741676244,1.),(1.,0.713722939843865,1.),(1.,0.71372400500128,
1.),(1.,0.71372556014432,1.),(1.,0.713723126099315,1.),(1.,0.713721352883477,
1.)))
REPRESENTATION_ITEM('')
SURFACE()
) ;
#38 = (
BOUNDED_SURFACE()
B_SPLINE_SURFACE(3,2,((#7638,#7639,#7640),(#7641,#7642,#7643),(#7644,#7645,
#7646),(#7647,#7648,#7649),(#7650,#7651,#7652),(#7653,#7654,#7655),(#7656,
#7657,#7658),(#7659,#7660,#7661),(#7662,#7663,#7664),(#7665,#7666,#7667),
(#7668,#7669,#7670),(#7671,#7672,#7673),(#7674,#7675,#7676),(#7677,#7678,
#7679),(#7680,#7681,#7682),(#7683,#7684,#7685),(#7686,#7687,#7688),(#7689,
#7690,#7691),(#7692,#7693,#7694),(#7695,#7696,#7697),(#7698,#7699,#7700),
(#7701,#7702,#7703),(#7704,#7705,#7706),(#7707,#7708,#7709),(#7710,#7711,
#7712),(#7713,#7714,#7715),(#7716,#7717,#7718),(#7719,#7720,#7721),(#7722,
#7723,#7724),(#7725,#7726,#7727),(#7728,#7729,#7730),(#7731,#7732,#7733),
(#7734,#7735,#7736),(#7737,#7738,#7739),(#7740,#7741,#7742),(#7743,#7744,
#7745)),.UNSPECIFIED.,.F.,.F.,.F.)
B_SPLINE_SURFACE_WITH_KNOTS((4,2,2,2,2,2,2,2,2,2,2,2,2,2,2,2,2,4),(3,3),
(0.110192674671804,0.119968567976379,0.129744461280954,0.139520354585529,
0.149296247890104,0.159072141194679,0.168848034499254,0.178623927803829,
0.183511874456117,0.188399821108404,0.198175714412979,0.207951607717554,
0.21772750102213,0.227503394326705,0.23727928763128,0.247055180935855,0.25683107424043,
0.266606967545005),(0.,1.),.UNSPECIFIED.)
GEOMETRIC_REPRESENTATION_ITEM()
RATIONAL_B_SPLINE_SURFACE(((1.,0.717557917014237,1.),(1.,0.717557424537029,
1.),(1.,0.717562701224584,1.),(1.,0.717561702784131,1.),(1.,0.717559005677598,
1.),(1.,0.717563327395298,1.),(1.,0.71756229102355,1.),(1.,0.717553816665384,
1.),(1.,0.717563248345556,1.),(1.,0.717560128435701,1.),(1.,0.717560865922022,
1.),(1.,0.717563079912224,1.),(1.,0.717555152410577,1.),(1.,0.717562714690268,
1.),(1.,0.71756327807233,1.),(1.,0.717559267698649,1.),(1.,0.71755827388903,
1.),(1.,0.717561484534412,1.),(1.,0.717562276061397,1.),(1.,0.717562227713511,
1.),(1.,0.717558058653909,1.),(1.,0.717563288912114,1.),(1.,0.717562675824823,
1.),(1.,0.717554973728334,1.),(1.,0.717563128966192,1.),(1.,0.717560719057696,
1.),(1.,0.717560347146644,1.),(1.,0.71756321785806,1.),(1.,0.717554301337103,
1.),(1.,0.717562479165266,1.),(1.,0.717563326012811,1.),(1.,0.717558566701041,
1.),(1.,0.717561980953627,1.),(1.,0.717562507334971,1.),(1.,0.717555378769111,
1.),(1.,0.717566078456109,1.)))
REPRESENTATION_ITEM('')
SURFACE()
) ;
#39 = (
BOUNDED_SURFACE()
B_SPLINE_SURFACE(1,2,((#7779,#7780,#7781,#7782,#7783,#7784,#7785,#7786,
#7787,#7788,#7789,#7790,#7791,#7792,#7793,#7794,#7795,#7796,#7797,#7798,
#7799,#7800,#7801),(#7802,#7803,#7804,#7805,#7806,#7807,#7808,#7809,#7810,
#7811,#7812,#7813,#7814,#7815,#7816,#7817,#7818,#7819,#7820,#7821,#7822,
#7823,#7824)),.UNSPECIFIED.,.F.,.F.,.F.)
B_SPLINE_SURFACE_WITH_KNOTS((2,2),(3,2,2,2,2,2,2,2,2,2,2,3),(0.,1.),(-1.03311088010868E-7,
0.0147058823529412,0.0294117647058824,0.0441176470588235,0.0588235294117647,
0.0735294117647059,0.0882352941176471,0.102941176470588,0.117647058823529,
0.132352941176471,0.147058823529412,0.159998951452637),.UNSPECIFIED.)
GEOMETRIC_REPRESENTATION_ITEM()
RATIONAL_B_SPLINE_SURFACE(((1.00000001499214,0.998932967306356,1.,0.998932974802372,
1.,0.998932974802372,1.,0.998932974802372,1.,0.998932974802372,1.,0.998932974802372,
1.,0.998932974802372,1.,0.998932974802372,1.,0.998932974802372,1.,0.998932974802372,
1.,0.999061093906287,0.999774528647208),(1.00000001499214,0.998932967306356,
1.,0.998932974802372,1.,0.998932974802372,1.,0.998932974802372,1.,0.998932974802372,
1.,0.998932974802372,1.,0.998932974802372,1.,0.998932974802372,1.,0.998932974802372,
1.,0.998932974802372,1.,0.999061093906287,0.999774528647208)))
REPRESENTATION_ITEM('')
SURFACE()
) ;
#40 = (
BOUNDED_SURFACE()
B_SPLINE_SURFACE(1,2,((#7968,#7969,#7970,#7971,#7972,#7973,#7974,#7975,
#7976,#7977,#7978,#7979,#7980,#7981,#7982,#7983,#7984,#7985,#7986,#7987,
#7988,#7989,#7990),(#7991,#7992,#7993,#7994,#7995,#7996,#7997,#7998,#7999,
#8000,#8001,#8002,#8003,#8004,#8005,#8006,#8007,#8008,#8009,#8010,#8011,
#8012,#8013)),.UNSPECIFIED.,.F.,.F.,.F.)
B_SPLINE_SURFACE_WITH_KNOTS((2,2),(3,2,2,2,2,2,2,2,2,2,2,3),(-2.12079722094204E-9,
1.),(-4.92610683626735E-10,0.0147058823529412,0.0294117647058824,0.0441176470588235,
0.0588235294117647,0.0735294117647059,0.0882352941176471,0.102941176470588,
0.117647058823529,0.132352941176471,0.147058823529412,0.159999479208712),
 .UNSPECIFIED.)
GEOMETRIC_REPRESENTATION_ITEM()
RATIONAL_B_SPLINE_SURFACE(((1.00000000007149,0.99893297476663,1.,0.998932974802373,
1.,0.998932974802373,1.,0.998932974802373,1.,0.998932974802373,1.,0.998932974802373,
1.,0.998932974802373,1.,0.998932974802373,1.,0.998932974802373,1.,0.998932974802373,
1.,0.999061055613513,0.999774586844051),(1.00000000007149,0.99893297476663,
1.,0.998932974802372,1.,0.998932974802372,1.,0.998932974802372,1.,0.998932974802372,
1.,0.998932974802372,1.,0.998932974802372,1.,0.998932974802372,1.,0.998932974802372,
1.,0.998932974802372,1.,0.999061055613513,0.999774586844051)))
REPRESENTATION_ITEM('')
SURFACE()
) ;
#41 = (
BOUNDED_SURFACE()
B_SPLINE_SURFACE(3,2,((#8180,#8181,#8182),(#8183,#8184,#8185),(#8186,#8187,
#8188),(#8189,#8190,#8191),(#8192,#8193,#8194),(#8195,#8196,#8197),(#8198,
#8199,#8200),(#8201,#8202,#8203),(#8204,#8205,#8206),(#8207,#8208,#8209),
(#8210,#8211,#8212),(#8213,#8214,#8215),(#8216,#8217,#8218),(#8219,#8220,
#8221),(#8222,#8223,#8224),(#8225,#8226,#8227),(#8228,#8229,#8230),(#8231,
#8232,#8233),(#8234,#8235,#8236),(#8237,#8238,#8239),(#8240,#8241,#8242),
(#8243,#8244,#8245),(#8246,#8247,#8248),(#8249,#8250,#8251),(#8252,#8253,
#8254),(#8255,#8256,#8257),(#8258,#8259,#8260),(#8261,#8262,#8263),(#8264,
#8265,#8266),(#8267,#8268,#8269),(#8270,#8271,#8272),(#8273,#8274,#8275)),
 .UNSPECIFIED.,.F.,.F.,.F.)
B_SPLINE_SURFACE_WITH_KNOTS((4,2,2,2,2,2,2,2,2,2,2,2,2,2,2,4),(3,3),(0.0363322941033848,
0.0552795959345893,0.0647532468501916,0.0742268977657939,0.0837005486813961,
0.0931741995969984,0.102647850512601,0.112121501428203,0.121595152343805,
0.131068803259407,0.14054245417501,0.150016105090612,0.159489756006214,
0.168963406921816,0.178437057837419,0.187910708753021),(0.,1.),
 .UNSPECIFIED.)
GEOMETRIC_REPRESENTATION_ITEM()
RATIONAL_B_SPLINE_SURFACE(((1.,0.713723577868358,1.),(1.,0.713722445286561,
1.),(1.,0.713725662290464,1.),(1.,0.713724573695348,1.),(1.,0.713722089511115,
1.),(1.,0.713725723127692,1.),(1.,0.713725237333952,1.),(1.,0.713719633277867,
1.),(1.,0.713725477122433,1.),(1.,0.713724228372051,1.),(1.,0.713722641353114,
1.),(1.,0.713725747753947,1.),(1.,0.713724999842608,1.),(1.,0.713718882715111,
1.),(1.,0.713725607168934,1.),(1.,0.713723850193677,1.),(1.,0.713723140210728,
1.),(1.,0.71372572998564,1.),(1.,0.713724718629055,1.),(1.,0.713718072404138,
1.),(1.,0.713725695723828,1.),(1.,0.713723420058332,1.),(1.,0.713723588633586,
1.),(1.,0.713725667937673,1.),(1.,0.713718399179848,1.),(1.,0.713724843886423,
1.),(1.,0.713725741689566,1.),(1.,0.713722939830535,1.),(1.,0.713724005000408,
1.),(1.,0.713725560145201,1.),(1.,0.71372312609865,1.),(1.,0.713721352883471,
1.)))
REPRESENTATION_ITEM('')
SURFACE()
) ;
#42 = (
BOUNDED_SURFACE()
B_SPLINE_SURFACE(3,2,((#8276,#8277,#8278),(#8279,#8280,#8281),(#8282,#8283,
#8284),(#8285,#8286,#8287),(#8288,#8289,#8290),(#8291,#8292,#8293),(#8294,
#8295,#8296),(#8297,#8298,#8299),(#8300,#8301,#8302),(#8303,#8304,#8305),
(#8306,#8307,#8308),(#8309,#8310,#8311),(#8312,#8313,#8314),(#8315,#8316,
#8317),(#8318,#8319,#8320),(#8321,#8322,#8323),(#8324,#8325,#8326),(#8327,
#8328,#8329),(#8330,#8331,#8332),(#8333,#8334,#8335),(#8336,#8337,#8338),
(#8339,#8340,#8341),(#8342,#8343,#8344),(#8345,#8346,#8347),(#8348,#8349,
#8350),(#8351,#8352,#8353),(#8354,#8355,#8356),(#8357,#8358,#8359),(#8360,
#8361,#8362),(#8363,#8364,#8365),(#8366,#8367,#8368),(#8369,#8370,#8371),
(#8372,#8373,#8374),(#8375,#8376,#8377),(#8378,#8379,#8380),(#8381,#8382,
#8383)),.UNSPECIFIED.,.F.,.F.,.F.)
B_SPLINE_SURFACE_WITH_KNOTS((4,2,2,2,2,2,2,2,2,2,2,2,2,2,2,2,2,4),(3,3),
(0.110192674671804,0.119968567976379,0.129744461280954,0.139520354585529,
0.149296247890104,0.159072141194679,0.168848034499254,0.178623927803829,
0.183511874456117,0.188399821108404,0.198175714412979,0.207951607717554,
0.21772750102213,0.227503394326705,0.23727928763128,0.247055180935855,0.25683107424043,
0.266606967545005),(0.,1.),.UNSPECIFIED.)
GEOMETRIC_REPRESENTATION_ITEM()
RATIONAL_B_SPLINE_SURFACE(((1.,0.717557917014254,1.),(1.,0.717557424547014,
1.),(1.,0.717562701211253,1.),(1.,0.717561702797474,1.),(1.,0.717559005695462,
1.),(1.,0.717563327377434,1.),(1.,0.71756229099605,1.),(1.,0.717553816692872,
1.),(1.,0.71756324839199,1.),(1.,0.717560128389276,1.),(1.,0.717560865954089,
1.),(1.,0.717563079880128,1.),(1.,0.717555152412765,1.),(1.,0.717562714688071,
1.),(1.,0.717563278030574,1.),(1.,0.717559267719585,1.),(1.,0.717558273903889,
1.),(1.,0.717561484519553,1.),(1.,0.717562276060567,1.),(1.,0.717562227715156,
1.),(1.,0.717558058640351,1.),(1.,0.717563288925658,1.),(1.,0.717562675824091,
1.),(1.,0.717554973729067,1.),(1.,0.717563128925084,1.),(1.,0.717560719098766,
1.),(1.,0.717560347141852,1.),(1.,0.717563217862797,1.),(1.,0.71755430134791,
1.),(1.,0.717562479154465,1.),(1.,0.717563326066472,1.),(1.,0.717558566647358,
1.),(1.,0.717561980967755,1.),(1.,0.717562507320847,1.),(1.,0.717555378779752,
1.),(1.,0.7175660784561,1.)))
REPRESENTATION_ITEM('')
SURFACE()
) ;
#43 = (
BOUNDED_SURFACE()
B_SPLINE_SURFACE(1,2,((#8416,#8417,#8418,#8419,#8420,#8421,#8422,#8423,
#8424,#8425,#8426,#8427,#8428,#8429,#8430,#8431,#8432,#8433,#8434,#8435,
#8436,#8437,#8438),(#8439,#8440,#8441,#8442,#8443,#8444,#8445,#8446,#8447,
#8448,#8449,#8450,#8451,#8452,#8453,#8454,#8455,#8456,#8457,#8458,#8459,
#8460,#8461)),.UNSPECIFIED.,.F.,.F.,.F.)
B_SPLINE_SURFACE_WITH_KNOTS((2,2),(3,2,2,2,2,2,2,2,2,2,2,3),(0.,1.),(-1.03311007440564E-7,
0.0147058823529412,0.0294117647058824,0.0441176470588235,0.0588235294117647,
0.0735294117647059,0.0882352941176471,0.102941176470588,0.117647058823529,
0.132352941176471,0.147058823529412,0.159998951452637),.UNSPECIFIED.)
GEOMETRIC_REPRESENTATION_ITEM()
RATIONAL_B_SPLINE_SURFACE(((1.00000001499213,0.998932967306362,1.,0.998932974802372,
1.,0.998932974802372,1.,0.998932974802372,1.,0.998932974802372,1.,0.998932974802372,
1.,0.998932974802372,1.,0.998932974802372,1.,0.998932974802372,1.,0.998932974802372,
1.,0.999061093906287,0.999774528647208),(1.00000001499213,0.998932967306362,
1.,0.998932974802372,1.,0.998932974802372,1.,0.998932974802372,1.,0.998932974802372,
1.,0.998932974802372,1.,0.998932974802372,1.,0.998932974802372,1.,0.998932974802372,
1.,0.998932974802372,1.,0.999061093906287,0.999774528647208)))
REPRESENTATION_ITEM('')
SURFACE()
) ;
#44 = (
BOUNDED_SURFACE()
B_SPLINE_SURFACE(1,2,((#8605,#8606,#8607,#8608,#8609,#8610,#8611,#8612,
#8613,#8614,#8615,#8616,#8617,#8618,#8619,#8620,#8621,#8622,#8623,#8624,
#8625,#8626,#8627),(#8628,#8629,#8630,#8631,#8632,#8633,#8634,#8635,#8636,
#8637,#8638,#8639,#8640,#8641,#8642,#8643,#8644,#8645,#8646,#8647,#8648,
#8649,#8650)),.UNSPECIFIED.,.F.,.F.,.F.)
B_SPLINE_SURFACE_WITH_KNOTS((2,2),(3,2,2,2,2,2,2,2,2,2,2,3),(-2.12079720203126E-9,
1.),(-4.92610607495987E-10,0.0147058823529412,0.0294117647058824,0.0441176470588235,
0.0588235294117647,0.0735294117647059,0.0882352941176471,0.102941176470588,
0.117647058823529,0.132352941176471,0.147058823529412,0.159999479208712),
 .UNSPECIFIED.)
GEOMETRIC_REPRESENTATION_ITEM()
RATIONAL_B_SPLINE_SURFACE(((1.00000000007148,0.998932974766629,1.,0.998932974802372,
1.,0.998932974802372,1.,0.998932974802372,1.,0.998932974802372,1.,0.998932974802372,
1.,0.998932974802372,1.,0.998932974802372,1.,0.998932974802372,1.,0.998932974802372,
1.,0.999061055613513,0.999774586844051),(1.00000000007149,0.99893297476663,
1.,0.998932974802372,1.,0.998932974802372,1.,0.998932974802372,1.,0.998932974802372,
1.,0.998932974802372,1.,0.998932974802372,1.,0.998932974802372,1.,0.998932974802372,
1.,0.998932974802372,1.,0.999061055613513,0.999774586844051)))
REPRESENTATION_ITEM('')
SURFACE()
) ;
#45 = (
BOUNDED_SURFACE()
B_SPLINE_SURFACE(3,2,((#8817,#8818,#8819),(#8820,#8821,#8822),(#8823,#8824,
#8825),(#8826,#8827,#8828),(#8829,#8830,#8831),(#8832,#8833,#8834),(#8835,
#8836,#8837),(#8838,#8839,#8840),(#8841,#8842,#8843),(#8844,#8845,#8846),
(#8847,#8848,#8849),(#8850,#8851,#8852),(#8853,#8854,#8855),(#8856,#8857,
#8858),(#8859,#8860,#8861),(#8862,#8863,#8864),(#8865,#8866,#8867),(#8868,
#8869,#8870),(#8871,#8872,#8873),(#8874,#8875,#8876),(#8877,#8878,#8879),
(#8880,#8881,#8882),(#8883,#8884,#8885),(#8886,#8887,#8888),(#8889,#8890,
#8891),(#8892,#8893,#8894),(#8895,#8896,#8897),(#8898,#8899,#8900),(#8901,
#8902,#8903),(#8904,#8905,#8906),(#8907,#8908,#8909),(#8910,#8911,#8912)),
 .UNSPECIFIED.,.F.,.F.,.F.)
B_SPLINE_SURFACE_WITH_KNOTS((4,2,2,2,2,2,2,2,2,2,2,2,2,2,2,4),(3,3),(0.0363322941033848,
0.0552795959345893,0.0647532468501916,0.0742268977657938,0.0837005486813961,
0.0931741995969983,0.102647850512601,0.112121501428203,0.121595152343805,
0.131068803259407,0.14054245417501,0.150016105090612,0.159489756006214,
0.168963406921816,0.178437057837419,0.187910708753021),(0.,1.),
 .UNSPECIFIED.)
GEOMETRIC_REPRESENTATION_ITEM()
RATIONAL_B_SPLINE_SURFACE(((1.,0.713723577868383,1.),(1.,0.713722445236779,
1.),(1.,0.713725662356741,1.),(1.,0.713724573662225,1.),(1.,0.713722089533019,
1.),(1.,0.713725723105761,1.),(1.,0.713725237328151,1.),(1.,0.713719633283652,
1.),(1.,0.713725477073128,1.),(1.,0.713724228421365,1.),(1.,0.713722641394657,
1.),(1.,0.713725747712396,1.),(1.,0.713724999816327,1.),(1.,0.713718882741423,
1.),(1.,0.713725607146823,1.),(1.,0.713723850215792,1.),(1.,0.713723140163847,
1.),(1.,0.71372573003249,1.),(1.,0.713724718644484,1.),(1.,0.71371807238871,
1.),(1.,0.713725695693675,1.),(1.,0.713723420088484,1.),(1.,0.713723588715348,
1.),(1.,0.713725667855899,1.),(1.,0.713718399201785,1.),(1.,0.713724843864469,
1.),(1.,0.71372574166801,1.),(1.,0.713722939852113,1.),(1.,0.71372400503284,
1.),(1.,0.713725560112773,1.),(1.,0.713723126123005,1.),(1.,0.713721352883481,
1.)))
REPRESENTATION_ITEM('')
SURFACE()
) ;
#46 = (
BOUNDED_SURFACE()
B_SPLINE_SURFACE(3,2,((#8913,#8914,#8915),(#8916,#8917,#8918),(#8919,#8920,
#8921),(#8922,#8923,#8924),(#8925,#8926,#8927),(#8928,#8929,#8930),(#8931,
#8932,#8933),(#8934,#8935,#8936),(#8937,#8938,#8939),(#8940,#8941,#8942),
(#8943,#8944,#8945),(#8946,#8947,#8948),(#8949,#8950,#8951),(#8952,#8953,
#8954),(#8955,#8956,#8957),(#8958,#8959,#8960),(#8961,#8962,#8963),(#8964,
#8965,#8966),(#8967,#8968,#8969),(#8970,#8971,#8972),(#8973,#8974,#8975),
(#8976,#8977,#8978),(#8979,#8980,#8981),(#8982,#8983,#8984),(#8985,#8986,
#8987),(#8988,#8989,#8990),(#8991,#8992,#8993),(#8994,#8995,#8996),(#8997,
#8998,#8999),(#9000,#9001,#9002),(#9003,#9004,#9005),(#9006,#9007,#9008),
(#9009,#9010,#9011),(#9012,#9013,#9014),(#9015,#9016,#9017),(#9018,#9019,
#9020)),.UNSPECIFIED.,.F.,.F.,.F.)
B_SPLINE_SURFACE_WITH_KNOTS((4,2,2,2,2,2,2,2,2,2,2,2,2,2,2,2,2,4),(3,3),
(0.110192674671804,0.119968567976379,0.129744461280954,0.139520354585529,
0.149296247890104,0.159072141194679,0.168848034499254,0.178623927803829,
0.183511874456117,0.188399821108404,0.198175714412979,0.207951607717554,
0.217727501022129,0.227503394326704,0.23727928763128,0.247055180935855,
0.25683107424043,0.266606967545005),(0.,1.00023388176495),.UNSPECIFIED.)
GEOMETRIC_REPRESENTATION_ITEM()
RATIONAL_B_SPLINE_SURFACE(((1.,0.717491858961397,1.00013214700528),(1.,
0.717491366381689,1.00013214723569),(1.,0.717496644273678,1.00013214476688),
(1.,0.717495645633698,1.00013214523401),(1.,0.717492947926026,1.0001321464959),
(1.,0.717497270561146,1.00013214447393),(1.,0.717496233954528,1.00013214495881),
(1.,0.717487757692677,1.0001321489237),(1.,0.717497191556528,1.00013214451089),
(1.,0.717494070883108,1.00013214597062),(1.,0.717494808582735,1.00013214562555),
(1.,0.71749702304298,1.0001321445897),(1.,0.717489093728662,1.00013214829875),
(1.,0.717496657741948,1.00013214476058),(1.,0.717497221266918,1.00013214449699),
(1.,0.71749320996491,1.00013214637333),(1.,0.717492215950634,1.00013214683829),
(1.,0.71749542728491,1.00013214533615),(1.,0.717496219027939,1.0001321449658),
(1.,0.717496170669021,1.00013214498842),(1.,0.717492000648466,1.000132146939),
(1.,0.717497232101359,1.00013214449192),(1.,0.717496618895965,1.00013214477875),
(1.,0.717488914976109,1.00013214838237),(1.,0.717497072114508,1.00013214456675),
(1.,0.717494661677973,1.00013214569427),(1.,0.717494289673323,1.00013214586828),
(1.,0.717497161033782,1.00013214452516),(1.,0.717488242471211,1.00013214869694),
(1.,0.717496422146812,1.00013214487079),(1.,0.717497269224653,1.00013214447455),
(1.,0.7174925088005,1.00013214670131),(1.,0.7174959238285,1.00013214510388),
(1.,0.717496450378461,1.00013214485758),(1.,0.717489320105511,1.00013214819286),
(1.,0.717500022312063,1.00013214318676)))
REPRESENTATION_ITEM('')
SURFACE()
) ;
#47 = (
BOUNDED_SURFACE()
B_SPLINE_SURFACE(1,2,((#9053,#9054,#9055,#9056,#9057,#9058,#9059,#9060,
#9061,#9062,#9063,#9064,#9065,#9066,#9067,#9068,#9069,#9070,#9071,#9072,
#9073,#9074,#9075),(#9076,#9077,#9078,#9079,#9080,#9081,#9082,#9083,#9084,
#9085,#9086,#9087,#9088,#9089,#9090,#9091,#9092,#9093,#9094,#9095,#9096,
#9097,#9098)),.UNSPECIFIED.,.F.,.F.,.F.)
B_SPLINE_SURFACE_WITH_KNOTS((2,2),(3,2,2,2,2,2,2,2,2,2,2,3),(0.,1.),(-1.0331090323905E-7,
0.0147058823529412,0.0294117647058824,0.0441176470588235,0.0588235294117647,
0.0735294117647059,0.0882352941176471,0.102941176470588,0.117647058823529,
0.132352941176471,0.147058823529412,0.159998951452637),.UNSPECIFIED.)
GEOMETRIC_REPRESENTATION_ITEM()
RATIONAL_B_SPLINE_SURFACE(((1.00000001499211,0.998932967306369,1.,0.998932974802372,
1.,0.998932974802372,1.,0.998932974802372,1.,0.998932974802372,1.,0.998932974802372,
1.,0.998932974802372,1.,0.998932974802372,1.,0.998932974802372,1.,0.998932974802372,
1.,0.999061093906287,0.999774528647208),(1.00000001499211,0.998932967306369,
1.,0.998932974802372,1.,0.998932974802372,1.,0.998932974802372,1.,0.998932974802372,
1.,0.998932974802372,1.,0.998932974802372,1.,0.998932974802372,1.,0.998932974802372,
1.,0.998932974802372,1.,0.999061093906287,0.999774528647208)))
REPRESENTATION_ITEM('')
SURFACE()
) ;
#48 = (
BOUNDED_SURFACE()
B_SPLINE_SURFACE(1,2,((#9242,#9243,#9244,#9245,#9246,#9247,#9248,#9249,
#9250,#9251,#9252,#9253,#9254,#9255,#9256,#9257,#9258,#9259,#9260,#9261,
#9262,#9263,#9264),(#9265,#9266,#9267,#9268,#9269,#9270,#9271,#9272,#9273,
#9274,#9275,#9276,#9277,#9278,#9279,#9280,#9281,#9282,#9283,#9284,#9285,
#9286,#9287)),.UNSPECIFIED.,.F.,.F.,.F.)
B_SPLINE_SURFACE_WITH_KNOTS((2,2),(3,2,2,2,2,2,2,2,2,2,2,3),(-2.12079799133641E-9,
1.),(-4.92610666765903E-10,0.0147058823529412,0.0294117647058824,0.0441176470588235,
0.0588235294117647,0.0735294117647059,0.0882352941176471,0.102941176470588,
0.117647058823529,0.132352941176471,0.147058823529412,0.159999479208712),
 .UNSPECIFIED.)
GEOMETRIC_REPRESENTATION_ITEM()
RATIONAL_B_SPLINE_SURFACE(((1.00000000007149,0.99893297476663,1.,0.998932974802372,
1.,0.998932974802372,1.,0.998932974802372,1.,0.998932974802372,1.,0.998932974802372,
1.,0.998932974802372,1.,0.998932974802372,1.,0.998932974802372,1.,0.998932974802372,
1.,0.999061055613513,0.999774586844051),(1.00000000007149,0.99893297476663,
1.,0.998932974802372,1.,0.998932974802372,1.,0.998932974802372,1.,0.998932974802372,
1.,0.998932974802372,1.,0.998932974802372,1.,0.998932974802372,1.,0.998932974802372,
1.,0.998932974802372,1.,0.999061055613513,0.999774586844051)))
REPRESENTATION_ITEM('')
SURFACE()
) ;
#49 = (
BOUNDED_SURFACE()
B_SPLINE_SURFACE(3,2,((#9454,#9455,#9456),(#9457,#9458,#9459),(#9460,#9461,
#9462),(#9463,#9464,#9465),(#9466,#9467,#9468),(#9469,#9470,#9471),(#9472,
#9473,#9474),(#9475,#9476,#9477),(#9478,#9479,#9480),(#9481,#9482,#9483),
(#9484,#9485,#9486),(#9487,#9488,#9489),(#9490,#9491,#9492),(#9493,#9494,
#9495),(#9496,#9497,#9498),(#9499,#9500,#9501),(#9502,#9503,#9504),(#9505,
#9506,#9507),(#9508,#9509,#9510),(#9511,#9512,#9513),(#9514,#9515,#9516),
(#9517,#9518,#9519),(#9520,#9521,#9522),(#9523,#9524,#9525),(#9526,#9527,
#9528),(#9529,#9530,#9531),(#9532,#9533,#9534),(#9535,#9536,#9537),(#9538,
#9539,#9540),(#9541,#9542,#9543),(#9544,#9545,#9546),(#9547,#9548,#9549)),
 .UNSPECIFIED.,.F.,.F.,.F.)
B_SPLINE_SURFACE_WITH_KNOTS((4,2,2,2,2,2,2,2,2,2,2,2,2,2,2,4),(3,3),(0.0363322941033848,
0.0552795959345893,0.0647532468501916,0.0742268977657939,0.0837005486813961,
0.0931741995969984,0.102647850512601,0.112121501428203,0.121595152343805,
0.131068803259407,0.14054245417501,0.150016105090612,0.159489756006214,
0.168963406921816,0.178437057837419,0.187910708753021),(0.,1.),
 .UNSPECIFIED.)
GEOMETRIC_REPRESENTATION_ITEM()
RATIONAL_B_SPLINE_SURFACE(((1.,0.713723577868383,1.),(1.,0.71372244524152,
1.),(1.,0.71372566235043,1.),(1.,0.713724573665381,1.),(1.,0.713722089517223,
1.),(1.,0.713725723121526,1.),(1.,0.713725237291428,1.),(1.,0.71371963332031,
1.),(1.,0.713725477049126,1.),(1.,0.713724228445444,1.),(1.,0.713722641365561,
1.),(1.,0.713725747741501,1.),(1.,0.713724999819642,1.),(1.,0.713718882738076,
1.),(1.,0.71372560714099,1.),(1.,0.713723850221543,1.),(1.,0.713723140170877,
1.),(1.,0.713725730025478,1.),(1.,0.713724718581176,1.),(1.,0.713718072451985,
1.),(1.,0.713725695588659,1.),(1.,0.713723420193482,1.),(1.,0.713723588743928,
1.),(1.,0.713725667827276,1.),(1.,0.713718399166187,1.),(1.,0.71372484390015,
1.),(1.,0.71372574176479,1.),(1.,0.713722939755319,1.),(1.,0.713724005027918,
1.),(1.,0.713725560117667,1.),(1.,0.713723126119328,1.),(1.,0.713721352883472,
1.)))
REPRESENTATION_ITEM('')
SURFACE()
) ;
#50 = (
BOUNDED_SURFACE()
B_SPLINE_SURFACE(3,2,((#9550,#9551,#9552),(#9553,#9554,#9555),(#9556,#9557,
#9558),(#9559,#9560,#9561),(#9562,#9563,#9564),(#9565,#9566,#9567),(#9568,
#9569,#9570),(#9571,#9572,#9573),(#9574,#9575,#9576),(#9577,#9578,#9579),
(#9580,#9581,#9582),(#9583,#9584,#9585),(#9586,#9587,#9588),(#9589,#9590,
#9591),(#9592,#9593,#9594),(#9595,#9596,#9597),(#9598,#9599,#9600),(#9601,
#9602,#9603),(#9604,#9605,#9606),(#9607,#9608,#9609),(#9610,#9611,#9612),
(#9613,#9614,#9615),(#9616,#9617,#9618),(#9619,#9620,#9621),(#9622,#9623,
#9624),(#9625,#9626,#9627),(#9628,#9629,#9630),(#9631,#9632,#9633),(#9634,
#9635,#9636),(#9637,#9638,#9639),(#9640,#9641,#9642),(#9643,#9644,#9645),
(#9646,#9647,#9648),(#9649,#9650,#9651),(#9652,#9653,#9654),(#9655,#9656,
#9657)),.UNSPECIFIED.,.F.,.F.,.F.)
B_SPLINE_SURFACE_WITH_KNOTS((4,2,2,2,2,2,2,2,2,2,2,2,2,2,2,2,2,4),(3,3),
(0.110192674671804,0.119968567976379,0.129744461280954,0.139520354585529,
0.149296247890104,0.159072141194679,0.168848034499254,0.178623927803829,
0.183511874456117,0.188399821108404,0.198175714412979,0.207951607717554,
0.217727501022129,0.227503394326705,0.23727928763128,0.247055180935855,
0.25683107424043,0.266606967545005),(0.,1.),.UNSPECIFIED.)
GEOMETRIC_REPRESENTATION_ITEM()
RATIONAL_B_SPLINE_SURFACE(((1.,0.717557917014258,1.),(1.,0.717557424560011,
1.),(1.,0.717562701193914,1.),(1.,0.717561702814847,1.),(1.,0.71755900564737,
1.),(1.,0.717563327425588,1.),(1.,0.717562291025758,1.),(1.,0.717553816663223,
1.),(1.,0.717563248329896,1.),(1.,0.717560128451358,1.),(1.,0.717560865886123,
1.),(1.,0.717563079948143,1.),(1.,0.717555152391406,1.),(1.,0.717562714709462,
1.),(1.,0.717563278031631,1.),(1.,0.717559267718992,1.),(1.,0.71755827387268,
1.),(1.,0.717561484550715,1.),(1.,0.717562276065883,1.),(1.,0.717562227704526,
1.),(1.,0.71755805869716,1.),(1.,0.71756328886893,1.),(1.,0.717562675764556,
1.),(1.,0.717554973788595,1.),(1.,0.717563128952974,1.),(1.,0.717560719070892,
1.),(1.,0.717560347081223,1.),(1.,0.717563217923494,1.),(1.,0.71755430141606,
1.),(1.,0.717562479086372,1.),(1.,0.717563326002921,1.),(1.,0.717558566710936,
1.),(1.,0.71756198091345,1.),(1.,0.717562507375146,1.),(1.,0.717555378738943,
1.),(1.,0.717566078456158,1.)))
REPRESENTATION_ITEM('')
SURFACE()
) ;
#51 = B_SPLINE_CURVE_WITH_KNOTS('',3,(#5793,#5794,#5795,#5796),
 .UNSPECIFIED.,.F.,.F.,(4,4),(0.149240959230156,0.155663525084362),
 .UNSPECIFIED.) ;
#52 = B_SPLINE_CURVE_WITH_KNOTS('',3,(#5805,#5806,#5807,#5808,#5809,#5810,
#5811,#5812,#5813,#5814,#5815,#5816,#5817,#5818,#5819,#5820,#5821,#5822,
#5823,#5824,#5825,#5826,#5827,#5828,#5829,#5830,#5831,#5832,#5833,#5834,
#5835,#5836,#5837,#5838,#5839,#5840,#5841,#5842,#5843,#5844,#5845,#5846,
#5847,#5848,#5849,#5850,#5851,#5852,#5853,#5854,#5855,#5856,#5857,#5858,
#5859,#5860),.UNSPECIFIED.,.F.,.F.,(4,2,2,2,2,2,2,2,2,2,2,2,2,2,2,2,2,2,
2,2,2,2,2,2,2,2,2,4),(0.,0.00731512878245589,0.00902075833180565,0.0167240727068727,
0.0180415166636113,0.0261381508744796,0.027062274995417,0.0355562466737043,
0.0360830333272226,0.0449741716251418,0.0451037916590283,0.0541245499908339,
0.0543919669055456,0.0631453083226396,0.0638099851771147,0.0721660666544452,
0.0732283939342589,0.0826464947664068,0.0902075833180562,0.0920641197300344,
0.0992283416498616,0.101482130305131,0.108249099981667,0.110900185947423,
0.120317603377353,0.126290616645278,0.129734235290266,0.14433212758977),
 .UNSPECIFIED.) ;
#53 = B_SPLINE_CURVE_WITH_KNOTS('',3,(#5862,#5863,#5864,#5865),
 .UNSPECIFIED.,.F.,.F.,(4,4),(-0.00866851853360736,0.),.UNSPECIFIED.) ;
#54 = B_SPLINE_CURVE_WITH_KNOTS('',3,(#5868,#5869,#5870,#5871,#5872,#5873,
#5874,#5875,#5876,#5877,#5878,#5879,#5880,#5881,#5882,#5883,#5884,#5885,
#5886,#5887,#5888,#5889,#5890,#5891,#5892,#5893,#5894,#5895,#5896,#5897,
#5898,#5899,#5900,#5901,#5902,#5903,#5904,#5905,#5906,#5907,#5908,#5909,
#5910,#5911,#5912,#5913,#5914,#5915,#5916,#5917,#5918,#5919,#5920,#5921,
#5922,#5923,#5924,#5925,#5926,#5927,#5928,#5929),.UNSPECIFIED.,.F.,.F.,
(4,2,2,2,2,2,2,2,2,2,2,2,2,2,2,2,2,2,2,2,2,2,2,2,2,2,2,2,2,2,4),(3.94956318998463E-8,
0.00891142814756958,0.00932755995188492,0.0186551199037698,0.0187613828160708,
0.0286110142999948,0.0373102398075393,0.0384607884393804,0.046637799759424,
0.0483108212289063,0.0559653597113087,0.0581608694451579,0.0652929196631934,
0.0680105025743505,0.0746204796150781,0.0778602470751006,0.0827853130796942,
0.0839480395669628,0.0877102729721427,0.0932755995188474,0.0975581095945039,
0.102603159470732,0.107402909010666,0.111930719422617,0.117245126652995,
0.121258279374501,0.127085194433039,0.130585839326386,0.136923514137084,
0.146760505439294,0.149240959230156),.UNSPECIFIED.) ;
#55 = B_SPLINE_CURVE_WITH_KNOTS('',3,(#5932,#5933,#5934,#5935,#5936,#5937,
#5938,#5939,#5940,#5941,#5942,#5943,#5944,#5945,#5946,#5947,#5948,#5949,
#5950,#5951),.UNSPECIFIED.,.F.,.F.,(4,2,2,2,2,2,2,2,2,4),(0.0897547274400454,
0.0920640826369811,0.101482011794833,0.103399078907256,0.110221254640862,
0.110900374996111,0.117043430374467,0.12031784279818,0.12973472062429,0.144332127589771),
 .UNSPECIFIED.) ;
#56 = B_SPLINE_CURVE_WITH_KNOTS('',3,(#5953,#5954,#5955,#5956),
 .UNSPECIFIED.,.F.,.F.,(4,4),(-0.0147595409796903,0.),.UNSPECIFIED.) ;
#57 = B_SPLINE_CURVE_WITH_KNOTS('',3,(#5960,#5961,#5962,#5963,#5964,#5965,
#5966,#5967,#5968,#5969,#5970,#5971,#5972,#5973,#5974,#5975,#5976,#5977),
 .UNSPECIFIED.,.F.,.F.,(4,2,2,2,2,2,2,2,4),(3.23478334301053E-8,0.00950796128231213,
0.0136581275144307,0.0258902720983011,0.0273162550288615,0.0409743825432922,
0.0474513189825906,0.0478034463005076,0.0546325100577231),.UNSPECIFIED.) ;
#58 = B_SPLINE_CURVE_WITH_KNOTS('',3,(#5979,#5980,#5981,#5982,#5983,#5984,
#5985,#5986,#5987,#5988,#5989,#5990,#5991,#5992,#5993,#5994,#5995,#5996,
#5997,#5998,#5999,#6000,#6001,#6002,#6003,#6004,#6005,#6006,#6007,#6008,
#6009,#6010,#6011,#6012,#6013,#6014,#6015,#6016,#6017,#6018,#6019,#6020,
#6021,#6022,#6023,#6024,#6025,#6026,#6027,#6028,#6029,#6030,#6031,#6032,
#6033,#6034,#6035,#6036,#6037,#6038,#6039),.UNSPECIFIED.,.F.,.F.,(4,3,3,
3,3,3,3,3,3,3,3,3,3,3,3,3,3,3,3,3,4),(0.0546325100577231,0.058160873912377,
0.067357759257812,0.0680104909370463,0.0778602344007145,0.0798902638143831,
0.0827851932736896,0.086204702253548,0.0877102855556224,0.0925191406927129,
0.0975581115684209,0.105148017571043,0.107402908109119,0.116343229848907,
0.117245131820784,0.127085188202925,0.130405771327702,0.136923515438958,
0.143034648206032,0.146760502503953,0.155663525084362),.UNSPECIFIED.) ;
#59 = B_SPLINE_CURVE_WITH_KNOTS('',3,(#6042,#6043,#6044,#6045,#6046,#6047,
#6048,#6049,#6050,#6051,#6052,#6053,#6054,#6055,#6056,#6057,#6058,#6059,
#6060,#6061,#6062,#6063,#6064,#6065,#6066,#6067,#6068,#6069,#6070,#6071,
#6072,#6073,#6074,#6075,#6076,#6077,#6078),.UNSPECIFIED.,.F.,.F.,(4,2,2,
2,2,2,2,2,2,3,2,2,2,2,2,2,2,4),(0.,0.00731512646279782,0.0112193409300058,
0.016724079282874,0.0224386818600116,0.0261380306119276,0.0336580227900174,
0.0355562890153248,0.0448773637200232,0.0449741716018943,0.0543919626298755,
0.0560967046500289,0.0638102284561295,0.0673160455800344,0.0732282109179109,
0.0785353865100399,0.0826463437232967,0.0897547274400454),.UNSPECIFIED.) ;
#60 = B_SPLINE_CURVE_WITH_KNOTS('',3,(#6081,#6082,#6083,#6084,#6085,#6086,
#6087,#6088,#6089,#6090,#6091,#6092,#6093,#6094,#6095,#6096,#6097,#6098,
#6099,#6100,#6101,#6102,#6103,#6104,#6105,#6106,#6107,#6108,#6109,#6110,
#6111,#6112,#6113,#6114,#6115,#6116,#6117,#6118,#6119,#6120,#6121,#6122,
#6123,#6124,#6125,#6126,#6127,#6128,#6129,#6130,#6131,#6132,#6133,#6134,
#6135,#6136),.UNSPECIFIED.,.F.,.F.,(4,2,2,2,2,2,2,2,2,2,2,2,2,2,2,2,2,2,
2,2,2,2,2,2,2,2,2,4),(0.,0.00731512878238814,0.00902075833180564,0.0167240727068785,
0.0180415166636113,0.0261381508744852,0.0270622749954169,0.0355562466737161,
0.0360830333272226,0.0449741716251424,0.0451037916590282,0.0541245499908339,
0.0543919669055449,0.0631453083226395,0.0638099851771106,0.0721660666544451,
0.0732283939342739,0.0826464947663908,0.0902075833180561,0.0920641197300239,
0.0992283416498616,0.101482130305075,0.108249099981667,0.110900185947284,
0.120317603377234,0.126290616645278,0.129734235290253,0.144332127589754),
 .UNSPECIFIED.) ;
#61 = B_SPLINE_CURVE_WITH_KNOTS('',3,(#6138,#6139,#6140,#6141),
 .UNSPECIFIED.,.F.,.F.,(4,4),(-0.0147606579860161,0.),.UNSPECIFIED.) ;
#62 = B_SPLINE_CURVE_WITH_KNOTS('',3,(#6145,#6146,#6147,#6148,#6149,#6150,
#6151,#6152,#6153,#6154,#6155,#6156,#6157,#6158,#6159,#6160,#6161,#6162,
#6163,#6164,#6165,#6166,#6167,#6168,#6169,#6170,#6171,#6172,#6173,#6174,
#6175,#6176,#6177,#6178,#6179,#6180,#6181,#6182,#6183,#6184,#6185,#6186,
#6187,#6188,#6189,#6190,#6191,#6192,#6193,#6194,#6195,#6196,#6197,#6198,
#6199,#6200,#6201,#6202,#6203,#6204,#6205,#6206,#6207,#6208),
 .UNSPECIFIED.,.F.,.F.,(4,2,2,2,2,2,2,2,2,2,2,2,2,3,2,3,2,2,2,2,2,2,2,2,
2,2,2,2,2,2,4),(3.94954787930727E-8,0.00891142512110372,0.00972897031777275,
0.0187613829416187,0.0194579406355455,0.028610894536375,0.0384607392810885,
0.0389158812710911,0.0483109273475211,0.0486448515888637,0.0581608647626506,
0.0583738219066363,0.0680105056195261,0.068102792224409,0.0778317625421816,
0.0778602325221652,0.0827853055179139,0.0875607328599542,0.0877103163614879,
0.0972897031777268,0.0975581136408448,0.107018673495499,0.107402909551261,
0.116747643813272,0.117245122911299,0.127085197251929,0.136205584448817,
0.136923529027027,0.14593455476659,0.146760502952475,0.155663525084362),
 .UNSPECIFIED.) ;
#63 = B_SPLINE_CURVE_WITH_KNOTS('',3,(#6212,#6213,#6214,#6215,#6216,#6217,
#6218,#6219,#6220,#6221,#6222,#6223,#6224,#6225,#6226,#6227,#6228,#6229,
#6230,#6231,#6232,#6233,#6234,#6235,#6236,#6237,#6238,#6239,#6240,#6241,
#6242,#6243,#6244,#6245,#6246,#6247,#6248,#6249,#6250,#6251,#6252,#6253,
#6254,#6255,#6256,#6257,#6258,#6259,#6260,#6261,#6262,#6263,#6264,#6265,
#6266,#6267,#6268),.UNSPECIFIED.,.F.,.F.,(4,2,2,2,2,2,2,2,2,2,3,2,2,2,2,
2,2,2,2,2,2,2,2,2,2,2,2,4),(0.,0.00731512878242812,0.00902075833180566,
0.016724072706909,0.0180415166636113,0.0261381508744844,0.027062274995417,
0.0355562466737159,0.0360830333272226,0.0449741716251424,0.0451037916590283,
0.054124549990834,0.0543919669055458,0.0631453083226396,0.0638099851771047,
0.0721660666544453,0.0732283939342734,0.0826464947662712,0.0902075833180563,
0.0920641197300701,0.0992283416498616,0.101482130305197,0.108249099981667,
0.110900185947437,0.120317603377343,0.126290616645278,0.129734235290238,
0.144332127589761),.UNSPECIFIED.) ;
#64 = B_SPLINE_CURVE_WITH_KNOTS('',3,(#6270,#6271,#6272,#6273),
 .UNSPECIFIED.,.F.,.F.,(4,4),(-0.0147606630153147,0.),.UNSPECIFIED.) ;
#65 = B_SPLINE_CURVE_WITH_KNOTS('',3,(#6277,#6278,#6279,#6280,#6281,#6282,
#6283,#6284,#6285,#6286,#6287,#6288,#6289,#6290,#6291,#6292,#6293,#6294,
#6295,#6296,#6297,#6298,#6299,#6300,#6301,#6302,#6303,#6304,#6305,#6306,
#6307,#6308,#6309,#6310,#6311,#6312,#6313,#6314,#6315,#6316,#6317,#6318,
#6319,#6320,#6321,#6322,#6323,#6324,#6325,#6326,#6327,#6328,#6329,#6330,
#6331,#6332,#6333,#6334,#6335,#6336,#6337,#6338,#6339),.UNSPECIFIED.,.F.,
 .F.,(4,2,2,2,2,2,2,2,2,2,2,2,2,2,2,3,2,2,2,2,2,2,2,2,2,2,2,2,2,2,4),(3.9495430696627E-8,
0.00891142512111904,0.00972897031777276,0.0187613829416347,0.0194579406355455,
0.028610894536505,0.0384607392810928,0.038915881271091,0.0483109273475251,
0.0486448515888636,0.0581608647626519,0.0583738219066362,0.0680105056195256,
0.0681027922244088,0.0778317625421815,0.0778602325221654,0.0827853055178527,
0.0875607328599541,0.0877103163614874,0.0972897031777267,0.0975581136408476,
0.107018673495499,0.107402909551269,0.116747643813272,0.117245122911301,
0.127085197251926,0.136205584448817,0.136923529027022,0.14593455476659,
0.146760502952473,0.155663525084362),.UNSPECIFIED.) ;
#66 = B_SPLINE_CURVE_WITH_KNOTS('',3,(#6343,#6344,#6345,#6346,#6347,#6348,
#6349,#6350,#6351,#6352,#6353,#6354,#6355,#6356,#6357,#6358,#6359,#6360,
#6361,#6362,#6363,#6364,#6365,#6366,#6367,#6368,#6369,#6370,#6371,#6372,
#6373,#6374,#6375,#6376,#6377,#6378,#6379,#6380,#6381,#6382,#6383,#6384,
#6385,#6386,#6387,#6388,#6389,#6390,#6391,#6392,#6393,#6394,#6395,#6396,
#6397,#6398),.UNSPECIFIED.,.F.,.F.,(4,2,2,2,2,2,2,2,2,2,2,2,2,2,2,2,2,2,
2,2,2,2,2,2,2,2,2,4),(0.,0.00731512878240043,0.00902075833180559,0.0167240727069339,
0.0180415166636112,0.0261381508744801,0.0270622749954168,0.0355562466737007,
0.0360830333272225,0.0449741716251419,0.0451037916590281,0.0541245499908337,
0.0543919669055447,0.0631453083226394,0.0638099851770966,0.072166066654445,
0.0732283939342627,0.0826464947664404,0.090207583318056,0.0920641197300776,
0.0992283416498613,0.101482130305149,0.108249099981667,0.110900185947403,
0.120317603377446,0.126290616645278,0.12973423529026,0.144332127589769),
 .UNSPECIFIED.) ;
#67 = B_SPLINE_CURVE_WITH_KNOTS('',3,(#6400,#6401,#6402,#6403),
 .UNSPECIFIED.,.F.,.F.,(4,4),(-0.00866852031690021,0.),.UNSPECIFIED.) ;
#68 = B_SPLINE_CURVE_WITH_KNOTS('',3,(#6407,#6408,#6409,#6410,#6411,#6412,
#6413,#6414,#6415,#6416,#6417,#6418,#6419,#6420,#6421,#6422,#6423,#6424,
#6425,#6426,#6427,#6428,#6429,#6430,#6431,#6432,#6433,#6434,#6435,#6436,
#6437,#6438,#6439,#6440,#6441,#6442,#6443,#6444,#6445,#6446,#6447,#6448,
#6449,#6450,#6451,#6452,#6453,#6454,#6455,#6456,#6457,#6458,#6459,#6460,
#6461,#6462,#6463,#6464,#6465,#6466,#6467,#6468,#6469),.UNSPECIFIED.,.F.,
 .F.,(4,2,2,2,2,2,2,2,2,2,2,2,2,2,2,3,2,2,2,2,2,2,2,2,2,2,2,2,2,2,4),(3.94954778143609E-8,
0.00891142512111536,0.00972897031777272,0.0187613829416454,0.0194579406355454,
0.0286108945365536,0.038460739281093,0.0389158812710909,0.0483109273475189,
0.0486448515888637,0.058160864762651,0.0583738219066364,0.068010505619526,
0.0681027922244092,0.077831762542182,0.0778602325221656,0.0827853055180071,
0.0875607328599548,0.0877103163614895,0.0972897031777276,0.0975581136408469,
0.1070186734955,0.107402909551265,0.116747643813273,0.1172451229113,0.127085197251908,
0.136205584448817,0.136923529027016,0.14593455476659,0.146760502952471,
0.155663525084362),.UNSPECIFIED.) ;
#69 = B_SPLINE_CURVE_WITH_KNOTS('',3,(#6475,#6476,#6477,#6478,#6479,#6480,
#6481,#6482,#6483,#6484,#6485,#6486),.UNSPECIFIED.,.F.,.F.,(4,2,2,2,2,4),
(-0.337170890175032,-0.295474578031491,-0.250449400518782,-0.168586531681465,
-0.0800191535060179,0.),.UNSPECIFIED.) ;
#70 = B_SPLINE_CURVE_WITH_KNOTS('',3,(#6488,#6489,#6490,#6491,#6492,#6493,
#6494,#6495,#6496,#6497,#6498,#6499),.UNSPECIFIED.,.F.,.F.,(4,2,2,2,2,4),
(-0.333222107964713,-0.254909679222191,-0.166608972895279,-0.0849984861950195,
-0.0408878594142492,0.),.UNSPECIFIED.) ;
#71 = B_SPLINE_CURVE_WITH_KNOTS('',3,(#6551,#6552,#6553,#6554,#6555,#6556),
 .UNSPECIFIED.,.F.,.F.,(4,2,4),(9.99999864681522E-7,7.73756153016491,14.6500515074066),
 .UNSPECIFIED.) ;
#72 = B_SPLINE_CURVE_WITH_KNOTS('',3,(#6557,#6558,#6559,#6560,#6561,#6562,
#6563,#6564,#6565,#6566,#6567,#6568,#6569,#6570,#6571,#6572,#6573,#6574,
#6575,#6576,#6577,#6578,#6579,#6580,#6581,#6582,#6583,#6584,#6585,#6586,
#6587,#6588,#6589,#6590,#6591,#6592,#6593,#6594,#6595,#6596,#6597,#6598,
#6599,#6600,#6601,#6602,#6603,#6604,#6605,#6606,#6607,#6608,#6609,#6610,
#6611,#6612,#6613,#6614,#6615,#6616,#6617,#6618,#6619,#6620,#6621,#6622,
#6623,#6624,#6625,#6626,#6627,#6628,#6629,#6630,#6631,#6632,#6633,#6634,
#6635,#6636,#6637,#6638,#6639,#6640,#6641,#6642,#6643,#6644),
 .UNSPECIFIED.,.F.,.F.,(4,3,3,3,3,3,3,3,3,3,3,3,3,3,3,3,3,3,3,3,3,3,3,3,
3,3,3,3,3,4),(0.,0.00937963669820284,0.0180867052587593,0.0187592733964057,
0.0275801848733995,0.0281389100946085,0.0370735108965404,0.0375185467928114,
0.0465678590763149,0.0468981834910142,0.0560614220554019,0.056277820189217,
0.0655556527434089,0.0750370935856226,0.0750489969011788,0.0844167302838255,
0.0845426524492584,0.0937963669820284,0.0940356196999413,0.103176003680231,
0.103530146128526,0.112555640378434,0.113023868907298,0.121935277076637,
0.122516583962713,0.13131491377484,0.132007368634961,0.140694550473043,
0.141493081370673,0.150074187171246),.UNSPECIFIED.) ;
#73 = B_SPLINE_CURVE_WITH_KNOTS('',3,(#6646,#6647,#6648,#6649,#6650,#6651,
#6652,#6653,#6654,#6655,#6656,#6657),.UNSPECIFIED.,.F.,.F.,(4,2,2,2,2,4),
(1.000000006113E-6,1.57108044003981,3.17385828869477,5.99475389679247,9.05882226516005,
11.9895252463837),.UNSPECIFIED.) ;
#74 = B_SPLINE_CURVE_WITH_KNOTS('',3,(#6678,#6679,#6680,#6681,#6682,#6683,
#6684,#6685,#6686,#6687,#6688,#6689,#6690,#6691),.UNSPECIFIED.,.F.,.F.,
(4,2,2,2,2,2,4),(3.16384028085258E-15,1.73074433286408,3.58539416576252,
6.63006684161914,9.43481733805421,11.4958871896749,13.2600099107559),
 .UNSPECIFIED.) ;
#75 = B_SPLINE_CURVE_WITH_KNOTS('',3,(#6739,#6740,#6741,#6742,#6743,#6744,
#6745,#6746,#6747,#6748,#6749,#6750,#6751,#6752,#6753,#6754,#6755,#6756,
#6757,#6758,#6759,#6760,#6761,#6762,#6763,#6764,#6765,#6766,#6767,#6768,
#6769,#6770,#6771,#6772,#6773,#6774,#6775,#6776,#6777,#6778,#6779,#6780,
#6781,#6782,#6783,#6784,#6785,#6786,#6787,#6788,#6789,#6790,#6791,#6792,
#6793,#6794,#6795,#6796,#6797,#6798,#6799,#6800,#6801,#6802,#6803,#6804,
#6805,#6806,#6807,#6808,#6809,#6810,#6811,#6812,#6813,#6814,#6815,#6816,
#6817,#6818),.UNSPECIFIED.,.F.,.F.,(4,2,2,2,2,2,2,2,2,2,2,2,2,2,2,2,2,2,
2,2,2,2,2,2,2,2,2,2,2,2,2,2,2,2,2,2,2,2,2,4),(-5.99999999998624E-8,0.000590526800461016,
0.00118111360092203,0.00236228720184421,0.00472463440368856,0.00769960210153364,
0.00944932880737708,0.0175309308941166,0.0188987176147543,0.0273655127101969,
0.0372020310641398,0.0377974952295087,0.0470416860700581,0.0472468840368859,
0.056696272844263,0.0568833874626172,0.0661456616516403,0.0667287422857246,
0.0716522046058592,0.0755950504590174,0.0765761128198491,0.086423531293351,
0.0944938280737717,0.0962698644460277,0.103943216881149,0.106117401685429,
0.113392605688526,0.115965067364374,0.122841994495903,0.125814419594229,
0.13229138330328,0.135667192159133,0.141740772110657,0.145521654063409,
0.146465466514346,0.14882781371619,0.150008786432466,0.150599272790603,
0.150760142698118,0.151189743027088),.UNSPECIFIED.) ;
#76 = B_SPLINE_CURVE_WITH_KNOTS('',3,(#6820,#6821,#6822,#6823,#6824,#6825),
 .UNSPECIFIED.,.F.,.F.,(4,2,4),(3.60319835854062E-5,9.64490115774811,19.2897662777575),
 .UNSPECIFIED.) ;
#77 = B_SPLINE_CURVE_WITH_KNOTS('',3,(#6827,#6828,#6829,#6830,#6831,#6832,
#6833,#6834,#6835,#6836,#6837,#6838,#6839,#6840),.UNSPECIFIED.,.F.,.F.,
(4,2,2,2,2,2,4),(1.00000002995617E-6,1.7692530094857,3.83875002010364,6.637598522414,
9.67546927736373,11.5382441958309,13.275259829094),.UNSPECIFIED.) ;
#78 = B_SPLINE_CURVE_WITH_KNOTS('',3,(#6857,#6858,#6859,#6860,#6861,#6862,
#6863,#6864,#6865,#6866,#6867,#6868,#6869,#6870),.UNSPECIFIED.,.F.,.F.,
(4,2,2,2,2,2,4),(9.99999993593914E-7,1.73146252564964,3.58437512441185,
6.6300673358595,9.43722227701482,11.4955951658395,13.2600876660263),
 .UNSPECIFIED.) ;
#79 = B_SPLINE_CURVE_WITH_KNOTS('',3,(#6878,#6879,#6880,#6881,#6882,#6883,
#6884,#6885,#6886,#6887,#6888,#6889),.UNSPECIFIED.,.F.,.F.,(4,2,2,2,2,4),
(1.45423920475118E-6,0.136695796634482,0.26996812895029,0.393732693444733,
0.460063012688564,0.516324865534141),.UNSPECIFIED.) ;
#80 = B_SPLINE_CURVE_WITH_KNOTS('',3,(#6890,#6891,#6892,#6893,#6894,#6895,
#6896,#6897,#6898,#6899,#6900,#6901,#6902,#6903),.UNSPECIFIED.,.F.,.F.,
(4,2,2,2,2,2,4),(0.,0.0210914408170582,0.0435982414579784,0.0952050288075531,
0.187105593312812,0.287813738176817,0.391818327243934),.UNSPECIFIED.) ;
#81 = B_SPLINE_CURVE_WITH_KNOTS('',3,(#7113,#7114,#7115,#7116,#7117,#7118,
#7119,#7120,#7121,#7122,#7123,#7124),.UNSPECIFIED.,.F.,.F.,(4,2,2,2,2,4),
(-0.337170890197259,-0.295474578044017,-0.250449400521991,-0.168586531692847,
-0.0800191535398783,0.),.UNSPECIFIED.) ;
#82 = B_SPLINE_CURVE_WITH_KNOTS('',3,(#7126,#7127,#7128,#7129,#7130,#7131,
#7132,#7133,#7134,#7135,#7136,#7137),.UNSPECIFIED.,.F.,.F.,(4,2,2,2,2,4),
(-0.333222107966658,-0.254909679269947,-0.166608972896623,-0.084998486132098,
-0.0408878593827511,0.),.UNSPECIFIED.) ;
#83 = B_SPLINE_CURVE_WITH_KNOTS('',3,(#7189,#7190,#7191,#7192,#7193,#7194),
 .UNSPECIFIED.,.F.,.F.,(4,2,4),(9.99999998905569E-7,7.73756066856093,14.6500505460067),
 .UNSPECIFIED.) ;
#84 = B_SPLINE_CURVE_WITH_KNOTS('',3,(#7195,#7196,#7197,#7198,#7199,#7200,
#7201,#7202,#7203,#7204,#7205,#7206,#7207,#7208,#7209,#7210,#7211,#7212,
#7213,#7214,#7215,#7216,#7217,#7218,#7219,#7220,#7221,#7222,#7223,#7224,
#7225,#7226,#7227,#7228,#7229,#7230,#7231,#7232,#7233,#7234,#7235,#7236,
#7237,#7238,#7239,#7240,#7241,#7242,#7243,#7244,#7245,#7246,#7247,#7248,
#7249,#7250,#7251,#7252,#7253,#7254,#7255,#7256,#7257,#7258,#7259,#7260,
#7261,#7262,#7263,#7264,#7265,#7266,#7267,#7268,#7269,#7270,#7271,#7272,
#7273,#7274,#7275,#7276,#7277,#7278,#7279,#7280,#7281,#7282),
 .UNSPECIFIED.,.F.,.F.,(4,3,3,3,3,3,3,3,3,3,3,3,3,3,3,3,3,3,3,3,3,3,3,3,
3,3,3,3,3,4),(0.,0.00937963669820301,0.0180867052587536,0.018759273396406,
0.0275801848734017,0.028138910094609,0.0370735108965484,0.037518546792812,
0.0465678590763189,0.046898183491015,0.0560614220554027,0.0562778201892181,
0.0655556527434121,0.0750370935856239,0.0750489969011802,0.0844167302838267,
0.0845426524492591,0.0937963669820294,0.0940356196999414,0.103176003680232,
0.103530146128525,0.112555640378435,0.113023868907291,0.121935277076638,
0.122516583962711,0.13131491377484,0.132007368634953,0.140694550473043,
0.141493081370687,0.150074187171246),.UNSPECIFIED.) ;
#85 = B_SPLINE_CURVE_WITH_KNOTS('',3,(#7284,#7285,#7286,#7287,#7288,#7289,
#7290,#7291,#7292,#7293,#7294,#7295),.UNSPECIFIED.,.F.,.F.,(4,2,2,2,2,4),
(1.00000001060884E-6,1.5710804400398,3.17385828869448,5.99475389679188,
9.05882226515939,11.9895252463828),.UNSPECIFIED.) ;
#86 = B_SPLINE_CURVE_WITH_KNOTS('',3,(#7316,#7317,#7318,#7319,#7320,#7321,
#7322,#7323,#7324,#7325,#7326,#7327,#7328,#7329),.UNSPECIFIED.,.F.,.F.,
(4,2,2,2,2,2,4),(4.9472447807214E-14,1.73074409285085,3.58539363528042,
6.630066337806,9.43481685331838,11.4958869837882,13.2600099122335),
 .UNSPECIFIED.) ;
#87 = B_SPLINE_CURVE_WITH_KNOTS('',3,(#7377,#7378,#7379,#7380,#7381,#7382,
#7383,#7384,#7385,#7386,#7387,#7388,#7389,#7390,#7391,#7392,#7393,#7394,
#7395,#7396,#7397,#7398,#7399,#7400,#7401,#7402,#7403,#7404,#7405,#7406,
#7407,#7408,#7409,#7410,#7411,#7412,#7413,#7414,#7415,#7416,#7417,#7418,
#7419,#7420,#7421,#7422,#7423,#7424,#7425,#7426,#7427,#7428,#7429,#7430,
#7431,#7432,#7433,#7434,#7435,#7436,#7437,#7438,#7439,#7440,#7441,#7442,
#7443,#7444,#7445,#7446,#7447,#7448,#7449,#7450,#7451,#7452,#7453,#7454,
#7455,#7456),.UNSPECIFIED.,.F.,.F.,(4,2,2,2,2,2,2,2,2,2,2,2,2,2,2,2,2,2,
2,2,2,2,2,2,2,2,2,2,2,2,2,2,2,2,2,2,2,2,2,4),(-5.99999999998624E-8,0.000590526800461144,
0.00118111360092229,0.00236228720184452,0.00472463440368883,0.0076996021015449,
0.00944932880737732,0.0175309308941572,0.0188987176147545,0.0273655127104135,
0.0372020310641432,0.0377974952295087,0.0470416860700603,0.0472468840368859,
0.056696272844263,0.0568833874626158,0.0661456616516401,0.0667287422857208,
0.071652204605778,0.0755950504590172,0.0765761128198549,0.0864235312935481,
0.0944938280737713,0.0962698644460535,0.103943216881148,0.106117401685444,
0.113392605688525,0.115965067364384,0.122841994495902,0.125814419594311,
0.132291383303279,0.135667192159198,0.141740772110656,0.145521654063392,
0.146465466514345,0.148827813716189,0.150008786432462,0.150599272790598,
0.150760142698139,0.151189743027081),.UNSPECIFIED.) ;
#88 = B_SPLINE_CURVE_WITH_KNOTS('',3,(#7458,#7459,#7460,#7461,#7462,#7463),
 .UNSPECIFIED.,.F.,.F.,(4,2,4),(3.60319838392225E-5,9.64490115776298,19.2897662777871),
 .UNSPECIFIED.) ;
#89 = B_SPLINE_CURVE_WITH_KNOTS('',3,(#7465,#7466,#7467,#7468,#7469,#7470,
#7471,#7472,#7473,#7474,#7475,#7476,#7477,#7478),.UNSPECIFIED.,.F.,.F.,
(4,2,2,2,2,2,4),(9.99999994089207E-7,1.76925387621149,3.83875073093921,
6.63759902241896,9.67546954853305,11.5382443266811,13.2752598290988),
 .UNSPECIFIED.) ;
#90 = B_SPLINE_CURVE_WITH_KNOTS('',3,(#7495,#7496,#7497,#7498,#7499,#7500,
#7501,#7502,#7503,#7504,#7505,#7506,#7507,#7508),.UNSPECIFIED.,.F.,.F.,
(4,2,2,2,2,2,4),(1.00000001476021E-6,1.73146252564982,3.58437512441194,
6.63006733585989,9.43722227701539,11.4955951658406,13.260087666028),
 .UNSPECIFIED.) ;
#91 = B_SPLINE_CURVE_WITH_KNOTS('',3,(#7516,#7517,#7518,#7519,#7520,#7521,
#7522,#7523,#7524,#7525,#7526,#7527),.UNSPECIFIED.,.F.,.F.,(4,2,2,2,2,4),
(9.99999888340319E-7,0.136552307695273,0.269611694582245,0.393232608950036,
0.459467944573314,0.515661056622118),.UNSPECIFIED.) ;
#92 = B_SPLINE_CURVE_WITH_KNOTS('',3,(#7528,#7529,#7530,#7531,#7532,#7533,
#7534,#7535,#7536,#7537,#7538,#7539,#7540,#7541),.UNSPECIFIED.,.F.,.F.,
(4,2,2,2,2,2,4),(0.,0.0210914408174009,0.0435982414581033,0.095205028809359,
0.187105593316175,0.287813738154874,0.391818327188839),.UNSPECIFIED.) ;
#93 = B_SPLINE_CURVE_WITH_KNOTS('',3,(#7751,#7752,#7753,#7754,#7755,#7756,
#7757,#7758,#7759,#7760,#7761,#7762),.UNSPECIFIED.,.F.,.F.,(4,2,2,2,2,4),
(-0.337170890186573,-0.295474578033596,-0.25044940051207,-0.168586531687245,
-0.08001915354066,0.),.UNSPECIFIED.) ;
#94 = B_SPLINE_CURVE_WITH_KNOTS('',3,(#7764,#7765,#7766,#7767,#7768,#7769,
#7770,#7771,#7772,#7773,#7774,#7775),.UNSPECIFIED.,.F.,.F.,(4,2,2,2,2,4),
(-0.333222107963772,-0.254909679273463,-0.166608972895298,-0.0849984861465236,
-0.0408878593888914,0.),.UNSPECIFIED.) ;
#95 = B_SPLINE_CURVE_WITH_KNOTS('',3,(#7827,#7828,#7829,#7830,#7831,#7832),
 .UNSPECIFIED.,.F.,.F.,(4,2,4),(9.99999977697379E-7,7.73756153014981,14.6500515071856),
 .UNSPECIFIED.) ;
#96 = B_SPLINE_CURVE_WITH_KNOTS('',3,(#7833,#7834,#7835,#7836,#7837,#7838,
#7839,#7840,#7841,#7842,#7843,#7844,#7845,#7846,#7847,#7848,#7849,#7850,
#7851,#7852,#7853,#7854,#7855,#7856,#7857,#7858,#7859,#7860,#7861,#7862,
#7863,#7864,#7865,#7866,#7867,#7868,#7869,#7870,#7871,#7872,#7873,#7874,
#7875,#7876,#7877,#7878,#7879,#7880,#7881,#7882,#7883,#7884,#7885,#7886,
#7887,#7888,#7889,#7890,#7891,#7892,#7893,#7894,#7895,#7896,#7897,#7898,
#7899,#7900,#7901,#7902,#7903,#7904,#7905,#7906,#7907,#7908,#7909,#7910,
#7911,#7912,#7913,#7914,#7915,#7916,#7917,#7918,#7919,#7920),
 .UNSPECIFIED.,.F.,.F.,(4,3,3,3,3,3,3,3,3,3,3,3,3,3,3,3,3,3,3,3,3,3,3,3,
3,3,3,3,3,4),(0.,0.00937963669820279,0.0180867052587558,0.0187592733964056,
0.0275801848734022,0.0281389100946084,0.0370735108965382,0.0375185467928111,
0.0465678590763102,0.0468981834910139,0.0560614220554001,0.0562778201892167,
0.0655556527434759,0.0750370935856223,0.0750489969011782,0.0844167302838252,
0.0845426524492568,0.0937963669820282,0.0940356196999407,0.103176003680231,
0.103530146128523,0.112555640378434,0.113023868907291,0.121935277076637,
0.122516583962714,0.13131491377484,0.132007368634949,0.140694550473043,
0.141493081370678,0.150074187171246),.UNSPECIFIED.) ;
#97 = B_SPLINE_CURVE_WITH_KNOTS('',3,(#7922,#7923,#7924,#7925,#7926,#7927,
#7928,#7929,#7930,#7931,#7932,#7933),.UNSPECIFIED.,.F.,.F.,(4,2,2,2,2,4),
(1.00000000092516E-6,1.57108130900177,3.17385902397466,5.99475439679111,
9.05882250959543,11.9895252463797),.UNSPECIFIED.) ;
#98 = B_SPLINE_CURVE_WITH_KNOTS('',3,(#7954,#7955,#7956,#7957,#7958,#7959,
#7960,#7961,#7962,#7963,#7964,#7965,#7966,#7967),.UNSPECIFIED.,.F.,.F.,
(4,2,2,2,2,2,4),(0.,1.73074422377745,3.58539390650711,6.63006683935466,
9.43481756703878,11.4958878534228,13.2600099122431),.UNSPECIFIED.) ;
#99 = B_SPLINE_CURVE_WITH_KNOTS('',3,(#8015,#8016,#8017,#8018,#8019,#8020,
#8021,#8022,#8023,#8024,#8025,#8026,#8027,#8028,#8029,#8030,#8031,#8032,
#8033,#8034,#8035,#8036,#8037,#8038,#8039,#8040,#8041,#8042,#8043,#8044,
#8045,#8046,#8047,#8048,#8049,#8050,#8051,#8052,#8053,#8054,#8055,#8056,
#8057,#8058,#8059,#8060,#8061,#8062,#8063,#8064,#8065,#8066,#8067,#8068,
#8069,#8070,#8071,#8072,#8073,#8074,#8075,#8076,#8077,#8078,#8079,#8080,
#8081,#8082,#8083,#8084,#8085,#8086,#8087,#8088,#8089,#8090,#8091,#8092,
#8093,#8094),.UNSPECIFIED.,.F.,.F.,(4,2,2,2,2,2,2,2,2,2,2,2,2,2,2,2,2,2,
2,2,2,2,2,2,2,2,2,2,2,2,2,2,2,2,2,2,2,2,2,4),(-5.99999999998624E-8,0.000590526800460891,
0.00118111360092178,0.00236228720184384,0.00472463440368797,0.00769960210153734,
0.0094493288073765,0.0175309308941643,0.0188987176147537,0.0273655127104343,
0.0372020310641408,0.037797495229508,0.0470416860700575,0.0472468840368852,
0.0566962728442623,0.0568833874626166,0.0661456616516395,0.0667287422857187,
0.0716522046058725,0.0755950504590167,0.0765761128198469,0.0864235312933632,
0.0944938280737709,0.0962698644460282,0.103943216881148,0.106117401685392,
0.113392605688525,0.11596506736434,0.122841994495902,0.125814419594224,
0.132291383303279,0.135667192159144,0.141740772110656,0.145521654063402,
0.146465466514345,0.148827813716189,0.150008786432464,0.150599272790601,
0.1507601426981,0.151189743027067),.UNSPECIFIED.) ;
#100 = B_SPLINE_CURVE_WITH_KNOTS('',3,(#8096,#8097,#8098,#8099,#8100,#8101),
 .UNSPECIFIED.,.F.,.F.,(4,2,4),(3.60319807248407E-5,9.64490115778259,19.2897662778294),
 .UNSPECIFIED.) ;
#101 = B_SPLINE_CURVE_WITH_KNOTS('',3,(#8103,#8104,#8105,#8106,#8107,#8108,
#8109,#8110,#8111,#8112,#8113,#8114,#8115,#8116),.UNSPECIFIED.,.F.,.F.,
(4,2,2,2,2,2,4),(1.0000000090877E-6,1.76925287661113,3.83874973180625,6.63759802391772,
9.67546855071821,11.5382433292875,13.2752598290998),.UNSPECIFIED.) ;
#102 = B_SPLINE_CURVE_WITH_KNOTS('',3,(#8133,#8134,#8135,#8136,#8137,#8138,
#8139,#8140,#8141,#8142,#8143,#8144,#8145,#8146),.UNSPECIFIED.,.F.,.F.,
(4,2,2,2,2,2,4),(1.00000000764925E-6,1.73146141725425,3.58437386659369,
6.63006633376183,9.43722150469471,11.4955948249276,13.2600876640189),
 .UNSPECIFIED.) ;
#103 = B_SPLINE_CURVE_WITH_KNOTS('',3,(#8154,#8155,#8156,#8157,#8158,#8159,
#8160,#8161,#8162,#8163,#8164,#8165),.UNSPECIFIED.,.F.,.F.,(4,2,2,2,2,4),
(9.99999885547778E-7,0.136552307551045,0.269611694272923,0.393232608587996,
0.459467944103502,0.515661056065258),.UNSPECIFIED.) ;
#104 = B_SPLINE_CURVE_WITH_KNOTS('',3,(#8166,#8167,#8168,#8169,#8170,#8171,
#8172,#8173,#8174,#8175,#8176,#8177,#8178,#8179),.UNSPECIFIED.,.F.,.F.,
(4,2,2,2,2,2,4),(0.,0.0210914408273525,0.0435982414795198,0.0952050288578533,
0.187105593300968,0.287813738141156,0.391818327182591),.UNSPECIFIED.) ;
#105 = B_SPLINE_CURVE_WITH_KNOTS('',3,(#8388,#8389,#8390,#8391,#8392,#8393,
#8394,#8395,#8396,#8397,#8398,#8399),.UNSPECIFIED.,.F.,.F.,(4,2,2,2,2,4),
(-0.337170890224052,-0.295474578066957,-0.250449400540881,-0.168586531705906,
-0.080019153547782,0.),.UNSPECIFIED.) ;
#106 = B_SPLINE_CURVE_WITH_KNOTS('',3,(#8401,#8402,#8403,#8404,#8405,#8406,
#8407,#8408,#8409,#8410,#8411,#8412),.UNSPECIFIED.,.F.,.F.,(4,2,2,2,2,4),
(-0.333222107941406,-0.254909678914244,-0.166608972882872,-0.0849984861480893,
-0.0408878594487005,0.),.UNSPECIFIED.) ;
#107 = B_SPLINE_CURVE_WITH_KNOTS('',3,(#8464,#8465,#8466,#8467,#8468,#8469),
 .UNSPECIFIED.,.F.,.F.,(4,2,4),(9.99999983881963E-7,7.73756066850657,14.6500505458332),
 .UNSPECIFIED.) ;
#108 = B_SPLINE_CURVE_WITH_KNOTS('',3,(#8470,#8471,#8472,#8473,#8474,#8475,
#8476,#8477,#8478,#8479,#8480,#8481,#8482,#8483,#8484,#8485,#8486,#8487,
#8488,#8489,#8490,#8491,#8492,#8493,#8494,#8495,#8496,#8497,#8498,#8499,
#8500,#8501,#8502,#8503,#8504,#8505,#8506,#8507,#8508,#8509,#8510,#8511,
#8512,#8513,#8514,#8515,#8516,#8517,#8518,#8519,#8520,#8521,#8522,#8523,
#8524,#8525,#8526,#8527,#8528,#8529,#8530,#8531,#8532,#8533,#8534,#8535,
#8536,#8537,#8538,#8539,#8540,#8541,#8542,#8543,#8544,#8545,#8546,#8547,
#8548,#8549,#8550,#8551,#8552,#8553,#8554,#8555,#8556,#8557),
 .UNSPECIFIED.,.F.,.F.,(4,3,3,3,3,3,3,3,3,3,3,3,3,3,3,3,3,3,3,3,3,3,3,3,
3,3,3,3,3,4),(0.,0.00937963669820289,0.0180867052587603,0.0187592733964058,
0.0275801848734026,0.0281389100946087,0.0370735108965375,0.0375185467928116,
0.0465678590763162,0.0468981834910144,0.0560614220554024,0.0562778201892173,
0.0655556527434056,0.0750370935856231,0.075048996901179,0.0844167302838259,
0.0845426524492572,0.0937963669820288,0.094035619699941,0.103176003680232,
0.103530146128528,0.112555640378434,0.113023868907299,0.121935277076637,
0.122516583962717,0.13131491377484,0.132007368634945,0.140694550473043,
0.141493081370679,0.150074187171246),.UNSPECIFIED.) ;
#109 = B_SPLINE_CURVE_WITH_KNOTS('',3,(#8559,#8560,#8561,#8562,#8563,#8564,
#8565,#8566,#8567,#8568,#8569,#8570),.UNSPECIFIED.,.F.,.F.,(4,2,2,2,2,4),
(9.99999976105999E-7,1.57108130900231,3.1738590239761,5.99475439679353,
9.05882250959927,11.9895252463846),.UNSPECIFIED.) ;
#110 = B_SPLINE_CURVE_WITH_KNOTS('',3,(#8591,#8592,#8593,#8594,#8595,#8596,
#8597,#8598,#8599,#8600,#8601,#8602,#8603,#8604),.UNSPECIFIED.,.F.,.F.,
(4,2,2,2,2,2,4),(0.,1.73074433286595,3.58539416576586,6.63006684162357,
9.43481733805997,11.4958871896815,13.2600099107624),.UNSPECIFIED.) ;
#111 = B_SPLINE_CURVE_WITH_KNOTS('',3,(#8652,#8653,#8654,#8655,#8656,#8657,
#8658,#8659,#8660,#8661,#8662,#8663,#8664,#8665,#8666,#8667,#8668,#8669,
#8670,#8671,#8672,#8673,#8674,#8675,#8676,#8677,#8678,#8679,#8680,#8681,
#8682,#8683,#8684,#8685,#8686,#8687,#8688,#8689,#8690,#8691,#8692,#8693,
#8694,#8695,#8696,#8697,#8698,#8699,#8700,#8701,#8702,#8703,#8704,#8705,
#8706,#8707,#8708,#8709,#8710,#8711,#8712,#8713,#8714,#8715,#8716,#8717,
#8718,#8719,#8720,#8721,#8722,#8723,#8724,#8725,#8726,#8727,#8728,#8729,
#8730,#8731),.UNSPECIFIED.,.F.,.F.,(4,2,2,2,2,2,2,2,2,2,2,2,2,2,2,2,2,2,
2,2,2,2,2,2,2,2,2,2,2,2,2,2,2,2,2,2,2,2,2,4),(-5.99999999998624E-8,0.000590526800461057,
0.00118111360092211,0.00236228720184423,0.00472463440368849,0.00769960210152361,
0.00944932880737713,0.0175309308941517,0.0188987176147546,0.0273655127104255,
0.0372020310641476,0.0377974952295093,0.0470416860700614,0.0472468840368866,
0.056696272844264,0.0568833874626169,0.0661456616516411,0.0667287422857187,
0.0716522046058997,0.0755950504590182,0.0765761128198413,0.0864235312933135,
0.0944938280737723,0.0962698644460061,0.103943216881149,0.106117401685439,
0.113392605688526,0.115965067364374,0.122841994495903,0.125814419594223,
0.13229138330328,0.135667192159117,0.141740772110657,0.14552165406341,0.146465466514345,
0.14882781371619,0.150008786432463,0.1505992727906,0.150760142698144,0.151189743027089),
 .UNSPECIFIED.) ;
#112 = B_SPLINE_CURVE_WITH_KNOTS('',3,(#8733,#8734,#8735,#8736,#8737,#8738),
 .UNSPECIFIED.,.F.,.F.,(4,2,4),(3.60319843423254E-5,9.64490065775652,19.2897662777735),
 .UNSPECIFIED.) ;
#113 = B_SPLINE_CURVE_WITH_KNOTS('',3,(#8740,#8741,#8742,#8743,#8744,#8745,
#8746,#8747,#8748,#8749,#8750,#8751,#8752,#8753),.UNSPECIFIED.,.F.,.F.,
(4,2,2,2,2,2,4),(1.00000000329695E-6,1.76925353789123,3.83874996049991,
6.63759802407595,9.67546829683264,11.5382432249431,13.2752598328519),
 .UNSPECIFIED.) ;
#114 = B_SPLINE_CURVE_WITH_KNOTS('',3,(#8770,#8771,#8772,#8773,#8774,#8775,
#8776,#8777,#8778,#8779,#8780,#8781,#8782,#8783),.UNSPECIFIED.,.F.,.F.,
(4,2,2,2,2,2,4),(9.99999971167725E-7,1.73146228667713,3.58437459628016,
6.63006683375916,9.43722179299249,11.4955949579948,13.2600876640179),
 .UNSPECIFIED.) ;
#115 = B_SPLINE_CURVE_WITH_KNOTS('',3,(#8791,#8792,#8793,#8794,#8795,#8796,
#8797,#8798,#8799,#8800,#8801,#8802),.UNSPECIFIED.,.F.,.F.,(4,2,2,2,2,4),
(9.99999764585794E-7,0.136553042381969,0.269612170499918,0.393232844695364,
0.459468051520106,0.515661054333012),.UNSPECIFIED.) ;
#116 = B_SPLINE_CURVE_WITH_KNOTS('',3,(#8803,#8804,#8805,#8806,#8807,#8808,
#8809,#8810,#8811,#8812,#8813,#8814,#8815,#8816),.UNSPECIFIED.,.F.,.F.,
(4,2,2,2,2,2,4),(0.,0.0210914409585585,0.0435982416633199,0.0952050281507284,
0.187105593156084,0.28781486856457,0.391819686950129),.UNSPECIFIED.) ;
#117 = B_SPLINE_CURVE_WITH_KNOTS('',3,(#9025,#9026,#9027,#9028,#9029,#9030,
#9031,#9032,#9033,#9034,#9035,#9036),.UNSPECIFIED.,.F.,.F.,(4,2,2,2,2,4),
(-0.337170890167228,-0.295474578027858,-0.250449400520224,-0.16858653167804,
-0.080019153500057,0.),.UNSPECIFIED.) ;
#118 = B_SPLINE_CURVE_WITH_KNOTS('',3,(#9038,#9039,#9040,#9041,#9042,#9043,
#9044,#9045,#9046,#9047,#9048,#9049),.UNSPECIFIED.,.F.,.F.,(4,2,2,2,2,4),
(-0.333222107943548,-0.254909679200476,-0.166608972885045,-0.084998486181255,
-0.0408878594089353,0.),.UNSPECIFIED.) ;
#119 = B_SPLINE_CURVE_WITH_KNOTS('',3,(#9101,#9102,#9103,#9104,#9105,#9106),
 .UNSPECIFIED.,.F.,.F.,(4,2,4),(9.99999993528995E-7,7.73756066846338,14.6500505457511),
 .UNSPECIFIED.) ;
#120 = B_SPLINE_CURVE_WITH_KNOTS('',3,(#9107,#9108,#9109,#9110,#9111,#9112,
#9113,#9114,#9115,#9116,#9117,#9118,#9119,#9120,#9121,#9122,#9123,#9124,
#9125,#9126,#9127,#9128,#9129,#9130,#9131,#9132,#9133,#9134,#9135,#9136,
#9137,#9138,#9139,#9140,#9141,#9142,#9143,#9144,#9145,#9146,#9147,#9148,
#9149,#9150,#9151,#9152,#9153,#9154,#9155,#9156,#9157,#9158,#9159,#9160,
#9161,#9162,#9163,#9164,#9165,#9166,#9167,#9168,#9169,#9170,#9171,#9172,
#9173,#9174,#9175,#9176,#9177,#9178,#9179,#9180,#9181,#9182,#9183,#9184,
#9185,#9186,#9187,#9188,#9189,#9190,#9191,#9192,#9193,#9194),
 .UNSPECIFIED.,.F.,.F.,(4,3,3,3,3,3,3,3,3,3,3,3,3,3,3,3,3,3,3,3,3,3,3,3,
3,3,3,3,3,4),(0.,0.00937963669820283,0.0180867052587627,0.0187592733964057,
0.0275801848734053,0.0281389100946085,0.0370735108965416,0.0375185467928113,
0.0465678590763129,0.0468981834910141,0.0560614220553998,0.056277820189217,
0.0655556527432504,0.0750370935856224,0.0750489969011785,0.0844167302838252,
0.0845426524492565,0.093796366982028,0.0940356196999399,0.103176003680231,
0.103530146128525,0.112555640378434,0.113023868907302,0.121935277076637,
0.122516583962714,0.13131491377484,0.132007368634939,0.140694550473043,
0.14149308137069,0.150074187171246),.UNSPECIFIED.) ;
#121 = B_SPLINE_CURVE_WITH_KNOTS('',3,(#9196,#9197,#9198,#9199,#9200,#9201,
#9202,#9203,#9204,#9205,#9206,#9207),.UNSPECIFIED.,.F.,.F.,(4,2,2,2,2,4),
(9.99999992923776E-7,1.57108130900183,3.17385902397465,5.99475439679217,
9.05882250959655,11.9895252463801),.UNSPECIFIED.) ;
#122 = B_SPLINE_CURVE_WITH_KNOTS('',3,(#9228,#9229,#9230,#9231,#9232,#9233,
#9234,#9235,#9236,#9237,#9238,#9239,#9240,#9241),.UNSPECIFIED.,.F.,.F.,
(4,2,2,2,2,2,4),(0.,1.7307444637883,3.58539443698107,6.63006734314984,9.43481805174913,
11.4958880592783,13.2600099107283),.UNSPECIFIED.) ;
#123 = B_SPLINE_CURVE_WITH_KNOTS('',3,(#9289,#9290,#9291,#9292,#9293,#9294,
#9295,#9296,#9297,#9298,#9299,#9300,#9301,#9302,#9303,#9304,#9305,#9306,
#9307,#9308,#9309,#9310,#9311,#9312,#9313,#9314,#9315,#9316,#9317,#9318,
#9319,#9320,#9321,#9322,#9323,#9324,#9325,#9326,#9327,#9328,#9329,#9330,
#9331,#9332,#9333,#9334,#9335,#9336,#9337,#9338,#9339,#9340,#9341,#9342,
#9343,#9344,#9345,#9346,#9347,#9348,#9349,#9350,#9351,#9352,#9353,#9354,
#9355,#9356,#9357,#9358,#9359,#9360,#9361,#9362,#9363,#9364,#9365,#9366,
#9367,#9368),.UNSPECIFIED.,.F.,.F.,(4,2,2,2,2,2,2,2,2,2,2,2,2,2,2,2,2,2,
2,2,2,2,2,2,2,2,2,2,2,2,2,2,2,2,2,2,2,2,2,4),(-5.99999999998624E-8,0.000590526800460957,
0.00118111360092191,0.00236228720184402,0.00472463440368833,0.00769960210154686,
0.0094493288073769,0.0175309308941876,0.0188987176147541,0.0273655127104106,
0.037202031064141,0.0377974952295082,0.0470416860700587,0.0472468840368852,
0.0566962728442623,0.0568833874626161,0.0661456616516395,0.0667287422857284,
0.0716522046057163,0.0755950504590167,0.0765761128198456,0.0864235312934359,
0.0944938280737711,0.0962698644460588,0.103943216881148,0.106117401685479,
0.113392605688525,0.115965067364307,0.122841994495902,0.125814419594179,
0.132291383303279,0.135667192159113,0.141740772110656,0.145521654063399,
0.146465466514345,0.148827813716189,0.150008786432465,0.150599272790602,
0.150760142698105,0.151189743027079),.UNSPECIFIED.) ;
#124 = B_SPLINE_CURVE_WITH_KNOTS('',3,(#9370,#9371,#9372,#9373,#9374,#9375),
 .UNSPECIFIED.,.F.,.F.,(4,2,4),(3.60319821137706E-5,9.64490115776887,19.2897662778005),
 .UNSPECIFIED.) ;
#125 = B_SPLINE_CURVE_WITH_KNOTS('',3,(#9377,#9378,#9379,#9380,#9381,#9382,
#9383,#9384,#9385,#9386,#9387,#9388,#9389,#9390),.UNSPECIFIED.,.F.,.F.,
(4,2,2,2,2,2,4),(9.99999999267761E-7,1.76925387621167,3.83875073094035,
6.63759902242126,9.67546954853661,11.5382443266855,13.2752598291039),
 .UNSPECIFIED.) ;
#126 = B_SPLINE_CURVE_WITH_KNOTS('',3,(#9407,#9408,#9409,#9410,#9411,#9412,
#9413,#9414,#9415,#9416,#9417,#9418,#9419,#9420),.UNSPECIFIED.,.F.,.F.,
(4,2,2,2,2,2,4),(1.00000000421862E-6,1.7314614172568,3.58437386659518,6.63006633376352,
9.43722150469613,11.4955948249291,13.2600876640204),.UNSPECIFIED.) ;
#127 = B_SPLINE_CURVE_WITH_KNOTS('',3,(#9428,#9429,#9430,#9431,#9432,#9433,
#9434,#9435,#9436,#9437,#9438,#9439),.UNSPECIFIED.,.F.,.F.,(4,2,2,2,2,4),
(1.45423872814327E-6,0.13669579668315,0.269968128958899,0.393732693269049,
0.460063012540498,0.516324865414279),.UNSPECIFIED.) ;
#128 = B_SPLINE_CURVE_WITH_KNOTS('',3,(#9440,#9441,#9442,#9443,#9444,#9445,
#9446,#9447,#9448,#9449,#9450,#9451,#9452,#9453),.UNSPECIFIED.,.F.,.F.,
(4,2,2,2,2,2,4),(0.,0.0210914408313759,0.0435982414838107,0.0952050288584094,
0.187105593266359,0.287813738105342,0.391818327152263),.UNSPECIFIED.) ;
#129 = CYLINDRICAL_SURFACE('',#4087,7.6) ;
#130 = CYLINDRICAL_SURFACE('',#4100,7.) ;
#131 = CYLINDRICAL_SURFACE('',#4101,35.0001428568513) ;
#132 = CYLINDRICAL_SURFACE('',#4102,7.) ;
#133 = CYLINDRICAL_SURFACE('',#4109,7.00000000000001) ;
#134 = CYLINDRICAL_SURFACE('',#4110,35.0001428568513) ;
#135 = CYLINDRICAL_SURFACE('',#4111,6.99999999999999) ;
#136 = CYLINDRICAL_SURFACE('',#4118,7.) ;
#137 = CYLINDRICAL_SURFACE('',#4119,35.0001428568513) ;
#138 = CYLINDRICAL_SURFACE('',#4120,7.) ;
#139 = CYLINDRICAL_SURFACE('',#4126,7.) ;
#140 = CYLINDRICAL_SURFACE('',#4127,35.0001428568513) ;
#141 = CYLINDRICAL_SURFACE('',#4128,7.) ;
#142 = CYLINDRICAL_SURFACE('',#4134,7.) ;
#143 = CYLINDRICAL_SURFACE('',#4135,35.0001428568513) ;
#144 = CYLINDRICAL_SURFACE('',#4136,6.99999999999999) ;
#145 = CYLINDRICAL_SURFACE('',#4139,35.75) ;
#146 = CYLINDRICAL_SURFACE('',#4142,35.9) ;
#147 = CYLINDRICAL_SURFACE('',#4162,2.) ;
#148 = CYLINDRICAL_SURFACE('',#4163,2.) ;
#149 = CYLINDRICAL_SURFACE('',#4164,2.) ;
#150 = CYLINDRICAL_SURFACE('',#4165,2.) ;
#151 = CYLINDRICAL_SURFACE('',#4171,41.0104872556708) ;
#152 = CYLINDRICAL_SURFACE('',#4186,0.549999999999984) ;
#153 = CYLINDRICAL_SURFACE('',#4187,0.4) ;
#154 = CYLINDRICAL_SURFACE('',#4199,0.549999999999995) ;
#155 = CYLINDRICAL_SURFACE('',#4200,0.4) ;
#156 = CYLINDRICAL_SURFACE('',#4212,0.549999999999995) ;
#157 = CYLINDRICAL_SURFACE('',#4213,0.399999999999995) ;
#158 = CYLINDRICAL_SURFACE('',#4225,0.550000000000001) ;
#159 = CYLINDRICAL_SURFACE('',#4226,0.4) ;
#160 = CYLINDRICAL_SURFACE('',#4275,0.600000000000001) ;
#161 = CYLINDRICAL_SURFACE('',#4276,0.600000000000001) ;
#162 = CYLINDRICAL_SURFACE('',#4277,0.599999999999996) ;
#163 = CYLINDRICAL_SURFACE('',#4278,0.600000000000001) ;
#164 = CYLINDRICAL_SURFACE('',#4279,0.600000000000001) ;
#165 = CYLINDRICAL_SURFACE('',#4280,0.600000000000001) ;
#166 = CYLINDRICAL_SURFACE('',#4281,0.599999999999996) ;
#167 = CYLINDRICAL_SURFACE('',#4282,0.600000000000001) ;
#168 = CYLINDRICAL_SURFACE('',#4326,0.600000000000001) ;
#169 = CYLINDRICAL_SURFACE('',#4327,0.600000000000001) ;
#170 = CYLINDRICAL_SURFACE('',#4328,0.599999999999996) ;
#171 = CYLINDRICAL_SURFACE('',#4329,0.600000000000001) ;
#172 = CYLINDRICAL_SURFACE('',#4330,0.600000000000001) ;
#173 = CYLINDRICAL_SURFACE('',#4331,0.600000000000001) ;
#174 = CYLINDRICAL_SURFACE('',#4332,0.599999999999996) ;
#175 = CYLINDRICAL_SURFACE('',#4333,0.600000000000001) ;
#176 = CYLINDRICAL_SURFACE('',#4377,0.600000000000001) ;
#177 = CYLINDRICAL_SURFACE('',#4378,0.600000000000001) ;
#178 = CYLINDRICAL_SURFACE('',#4379,0.599999999999997) ;
#179 = CYLINDRICAL_SURFACE('',#4380,0.600000000000001) ;
#180 = CYLINDRICAL_SURFACE('',#4381,0.600000000000001) ;
#181 = CYLINDRICAL_SURFACE('',#4382,0.600000000000001) ;
#182 = CYLINDRICAL_SURFACE('',#4383,0.599999999999997) ;
#183 = CYLINDRICAL_SURFACE('',#4384,0.600000000000001) ;
#184 = CYLINDRICAL_SURFACE('',#4428,0.600000000000001) ;
#185 = CYLINDRICAL_SURFACE('',#4429,0.600000000000001) ;
#186 = CYLINDRICAL_SURFACE('',#4430,0.599999999999996) ;
#187 = CYLINDRICAL_SURFACE('',#4431,0.600000000000001) ;
#188 = CYLINDRICAL_SURFACE('',#4432,0.600000000000001) ;
#189 = CYLINDRICAL_SURFACE('',#4433,0.600000000000001) ;
#190 = CYLINDRICAL_SURFACE('',#4434,0.599999999999996) ;
#191 = CYLINDRICAL_SURFACE('',#4435,0.600000000000001) ;
#192 = ITEM_DEFINED_TRANSFORMATION($,$,#3945,#4061) ;
#193 = ITEM_DEFINED_TRANSFORMATION($,$,#3958,#4062) ;
#194 = ITEM_DEFINED_TRANSFORMATION($,$,#3973,#4063) ;
#195 = ITEM_DEFINED_TRANSFORMATION($,$,#3977,#4064) ;
#196 = ITEM_DEFINED_TRANSFORMATION($,$,#3981,#4065) ;
#197 = ITEM_DEFINED_TRANSFORMATION($,$,#3985,#4066) ;
#198 = ITEM_DEFINED_TRANSFORMATION($,$,#3989,#4067) ;
#199 = ITEM_DEFINED_TRANSFORMATION($,$,#3993,#4068) ;
#200 = ITEM_DEFINED_TRANSFORMATION($,$,#3997,#4069) ;
#201 = ITEM_DEFINED_TRANSFORMATION($,$,#4001,#4070) ;
#202 = ITEM_DEFINED_TRANSFORMATION($,$,#4005,#4071) ;
#203 = ITEM_DEFINED_TRANSFORMATION($,$,#4009,#4072) ;
#204 = ITEM_DEFINED_TRANSFORMATION($,$,#4013,#4073) ;
#205 = ITEM_DEFINED_TRANSFORMATION($,$,#4017,#4074) ;
#206 = ITEM_DEFINED_TRANSFORMATION($,$,#4021,#4075) ;
#207 = ITEM_DEFINED_TRANSFORMATION($,$,#4025,#4076) ;
#208 = ITEM_DEFINED_TRANSFORMATION($,$,#4029,#4077) ;
#209 = ITEM_DEFINED_TRANSFORMATION($,$,#4033,#4078) ;
#210 = ITEM_DEFINED_TRANSFORMATION($,$,#4037,#4079) ;
#211 = ITEM_DEFINED_TRANSFORMATION($,$,#4041,#4080) ;
#212 = ITEM_DEFINED_TRANSFORMATION($,$,#4045,#4081) ;
#213 = ITEM_DEFINED_TRANSFORMATION($,$,#4049,#4082) ;
#214 = ITEM_DEFINED_TRANSFORMATION($,$,#4053,#4083) ;
#215 = ITEM_DEFINED_TRANSFORMATION($,$,#4057,#4084) ;
#216 = ITEM_DEFINED_TRANSFORMATION($,$,#4086,#4166) ;
#217 = ITEM_DEFINED_TRANSFORMATION($,$,#4138,#4167) ;
#218 = ITEM_DEFINED_TRANSFORMATION($,$,#4147,#4168) ;
#219 = ITEM_DEFINED_TRANSFORMATION($,$,#4170,#4436) ;
#220 = ITEM_DEFINED_TRANSFORMATION($,$,#4232,#4437) ;
#221 = ITEM_DEFINED_TRANSFORMATION($,$,#4283,#4438) ;
#222 = ITEM_DEFINED_TRANSFORMATION($,$,#4334,#4439) ;
#223 = ITEM_DEFINED_TRANSFORMATION($,$,#4385,#4440) ;
#224 = ITEM_DEFINED_TRANSFORMATION($,$,#3944,#4441) ;
#225 = ITEM_DEFINED_TRANSFORMATION($,$,#4085,#4442) ;
#226 = ITEM_DEFINED_TRANSFORMATION($,$,#4169,#4443) ;
#227 = (
REPRESENTATION_RELATIONSHIP($,$,#10448,#10447)
REPRESENTATION_RELATIONSHIP_WITH_TRANSFORMATION(#192)
SHAPE_REPRESENTATION_RELATIONSHIP()
) ;
#228 = (
REPRESENTATION_RELATIONSHIP($,$,#10449,#10447)
REPRESENTATION_RELATIONSHIP_WITH_TRANSFORMATION(#193)
SHAPE_REPRESENTATION_RELATIONSHIP()
) ;
#229 = (
REPRESENTATION_RELATIONSHIP($,$,#10450,#10447)
REPRESENTATION_RELATIONSHIP_WITH_TRANSFORMATION(#194)
SHAPE_REPRESENTATION_RELATIONSHIP()
) ;
#230 = (
REPRESENTATION_RELATIONSHIP($,$,#10451,#10447)
REPRESENTATION_RELATIONSHIP_WITH_TRANSFORMATION(#195)
SHAPE_REPRESENTATION_RELATIONSHIP()
) ;
#231 = (
REPRESENTATION_RELATIONSHIP($,$,#10452,#10447)
REPRESENTATION_RELATIONSHIP_WITH_TRANSFORMATION(#196)
SHAPE_REPRESENTATION_RELATIONSHIP()
) ;
#232 = (
REPRESENTATION_RELATIONSHIP($,$,#10453,#10447)
REPRESENTATION_RELATIONSHIP_WITH_TRANSFORMATION(#197)
SHAPE_REPRESENTATION_RELATIONSHIP()
) ;
#233 = (
REPRESENTATION_RELATIONSHIP($,$,#10454,#10447)
REPRESENTATION_RELATIONSHIP_WITH_TRANSFORMATION(#198)
SHAPE_REPRESENTATION_RELATIONSHIP()
) ;
#234 = (
REPRESENTATION_RELATIONSHIP($,$,#10455,#10447)
REPRESENTATION_RELATIONSHIP_WITH_TRANSFORMATION(#199)
SHAPE_REPRESENTATION_RELATIONSHIP()
) ;
#235 = (
REPRESENTATION_RELATIONSHIP($,$,#10456,#10447)
REPRESENTATION_RELATIONSHIP_WITH_TRANSFORMATION(#200)
SHAPE_REPRESENTATION_RELATIONSHIP()
) ;
#236 = (
REPRESENTATION_RELATIONSHIP($,$,#10457,#10447)
REPRESENTATION_RELATIONSHIP_WITH_TRANSFORMATION(#201)
SHAPE_REPRESENTATION_RELATIONSHIP()
) ;
#237 = (
REPRESENTATION_RELATIONSHIP($,$,#10458,#10447)
REPRESENTATION_RELATIONSHIP_WITH_TRANSFORMATION(#202)
SHAPE_REPRESENTATION_RELATIONSHIP()
) ;
#238 = (
REPRESENTATION_RELATIONSHIP($,$,#10459,#10447)
REPRESENTATION_RELATIONSHIP_WITH_TRANSFORMATION(#203)
SHAPE_REPRESENTATION_RELATIONSHIP()
) ;
#239 = (
REPRESENTATION_RELATIONSHIP($,$,#10460,#10447)
REPRESENTATION_RELATIONSHIP_WITH_TRANSFORMATION(#204)
SHAPE_REPRESENTATION_RELATIONSHIP()
) ;
#240 = (
REPRESENTATION_RELATIONSHIP($,$,#10461,#10447)
REPRESENTATION_RELATIONSHIP_WITH_TRANSFORMATION(#205)
SHAPE_REPRESENTATION_RELATIONSHIP()
) ;
#241 = (
REPRESENTATION_RELATIONSHIP($,$,#10462,#10447)
REPRESENTATION_RELATIONSHIP_WITH_TRANSFORMATION(#206)
SHAPE_REPRESENTATION_RELATIONSHIP()
) ;
#242 = (
REPRESENTATION_RELATIONSHIP($,$,#10463,#10447)
REPRESENTATION_RELATIONSHIP_WITH_TRANSFORMATION(#207)
SHAPE_REPRESENTATION_RELATIONSHIP()
) ;
#243 = (
REPRESENTATION_RELATIONSHIP($,$,#10464,#10447)
REPRESENTATION_RELATIONSHIP_WITH_TRANSFORMATION(#208)
SHAPE_REPRESENTATION_RELATIONSHIP()
) ;
#244 = (
REPRESENTATION_RELATIONSHIP($,$,#10465,#10447)
REPRESENTATION_RELATIONSHIP_WITH_TRANSFORMATION(#209)
SHAPE_REPRESENTATION_RELATIONSHIP()
) ;
#245 = (
REPRESENTATION_RELATIONSHIP($,$,#10466,#10447)
REPRESENTATION_RELATIONSHIP_WITH_TRANSFORMATION(#210)
SHAPE_REPRESENTATION_RELATIONSHIP()
) ;
#246 = (
REPRESENTATION_RELATIONSHIP($,$,#10467,#10447)
REPRESENTATION_RELATIONSHIP_WITH_TRANSFORMATION(#211)
SHAPE_REPRESENTATION_RELATIONSHIP()
) ;
#247 = (
REPRESENTATION_RELATIONSHIP($,$,#10468,#10447)
REPRESENTATION_RELATIONSHIP_WITH_TRANSFORMATION(#212)
SHAPE_REPRESENTATION_RELATIONSHIP()
) ;
#248 = (
REPRESENTATION_RELATIONSHIP($,$,#10469,#10447)
REPRESENTATION_RELATIONSHIP_WITH_TRANSFORMATION(#213)
SHAPE_REPRESENTATION_RELATIONSHIP()
) ;
#249 = (
REPRESENTATION_RELATIONSHIP($,$,#10470,#10447)
REPRESENTATION_RELATIONSHIP_WITH_TRANSFORMATION(#214)
SHAPE_REPRESENTATION_RELATIONSHIP()
) ;
#250 = (
REPRESENTATION_RELATIONSHIP($,$,#10471,#10447)
REPRESENTATION_RELATIONSHIP_WITH_TRANSFORMATION(#215)
SHAPE_REPRESENTATION_RELATIONSHIP()
) ;
#251 = (
REPRESENTATION_RELATIONSHIP($,$,#10473,#10472)
REPRESENTATION_RELATIONSHIP_WITH_TRANSFORMATION(#216)
SHAPE_REPRESENTATION_RELATIONSHIP()
) ;
#252 = (
REPRESENTATION_RELATIONSHIP($,$,#10474,#10472)
REPRESENTATION_RELATIONSHIP_WITH_TRANSFORMATION(#217)
SHAPE_REPRESENTATION_RELATIONSHIP()
) ;
#253 = (
REPRESENTATION_RELATIONSHIP($,$,#10475,#10472)
REPRESENTATION_RELATIONSHIP_WITH_TRANSFORMATION(#218)
SHAPE_REPRESENTATION_RELATIONSHIP()
) ;
#254 = (
REPRESENTATION_RELATIONSHIP($,$,#10477,#10476)
REPRESENTATION_RELATIONSHIP_WITH_TRANSFORMATION(#219)
SHAPE_REPRESENTATION_RELATIONSHIP()
) ;
#255 = (
REPRESENTATION_RELATIONSHIP($,$,#10478,#10476)
REPRESENTATION_RELATIONSHIP_WITH_TRANSFORMATION(#220)
SHAPE_REPRESENTATION_RELATIONSHIP()
) ;
#256 = (
REPRESENTATION_RELATIONSHIP($,$,#10479,#10476)
REPRESENTATION_RELATIONSHIP_WITH_TRANSFORMATION(#221)
SHAPE_REPRESENTATION_RELATIONSHIP()
) ;
#257 = (
REPRESENTATION_RELATIONSHIP($,$,#10480,#10476)
REPRESENTATION_RELATIONSHIP_WITH_TRANSFORMATION(#222)
SHAPE_REPRESENTATION_RELATIONSHIP()
) ;
#258 = (
REPRESENTATION_RELATIONSHIP($,$,#10481,#10476)
REPRESENTATION_RELATIONSHIP_WITH_TRANSFORMATION(#223)
SHAPE_REPRESENTATION_RELATIONSHIP()
) ;
#259 = (
REPRESENTATION_RELATIONSHIP($,$,#10447,#10446)
REPRESENTATION_RELATIONSHIP_WITH_TRANSFORMATION(#224)
SHAPE_REPRESENTATION_RELATIONSHIP()
) ;
#260 = (
REPRESENTATION_RELATIONSHIP($,$,#10472,#10446)
REPRESENTATION_RELATIONSHIP_WITH_TRANSFORMATION(#225)
SHAPE_REPRESENTATION_RELATIONSHIP()
) ;
#261 = (
REPRESENTATION_RELATIONSHIP($,$,#10476,#10446)
REPRESENTATION_RELATIONSHIP_WITH_TRANSFORMATION(#226)
SHAPE_REPRESENTATION_RELATIONSHIP()
) ;
#262 = CONTEXT_DEPENDENT_SHAPE_REPRESENTATION(#227,#10401) ;
#263 = CONTEXT_DEPENDENT_SHAPE_REPRESENTATION(#228,#10402) ;
#264 = CONTEXT_DEPENDENT_SHAPE_REPRESENTATION(#229,#10403) ;
#265 = CONTEXT_DEPENDENT_SHAPE_REPRESENTATION(#230,#10404) ;
#266 = CONTEXT_DEPENDENT_SHAPE_REPRESENTATION(#231,#10405) ;
#267 = CONTEXT_DEPENDENT_SHAPE_REPRESENTATION(#232,#10406) ;
#268 = CONTEXT_DEPENDENT_SHAPE_REPRESENTATION(#233,#10407) ;
#269 = CONTEXT_DEPENDENT_SHAPE_REPRESENTATION(#234,#10408) ;
#270 = CONTEXT_DEPENDENT_SHAPE_REPRESENTATION(#235,#10409) ;
#271 = CONTEXT_DEPENDENT_SHAPE_REPRESENTATION(#236,#10410) ;
#272 = CONTEXT_DEPENDENT_SHAPE_REPRESENTATION(#237,#10411) ;
#273 = CONTEXT_DEPENDENT_SHAPE_REPRESENTATION(#238,#10412) ;
#274 = CONTEXT_DEPENDENT_SHAPE_REPRESENTATION(#239,#10413) ;
#275 = CONTEXT_DEPENDENT_SHAPE_REPRESENTATION(#240,#10414) ;
#276 = CONTEXT_DEPENDENT_SHAPE_REPRESENTATION(#241,#10415) ;
#277 = CONTEXT_DEPENDENT_SHAPE_REPRESENTATION(#242,#10416) ;
#278 = CONTEXT_DEPENDENT_SHAPE_REPRESENTATION(#243,#10417) ;
#279 = CONTEXT_DEPENDENT_SHAPE_REPRESENTATION(#244,#10418) ;
#280 = CONTEXT_DEPENDENT_SHAPE_REPRESENTATION(#245,#10419) ;
#281 = CONTEXT_DEPENDENT_SHAPE_REPRESENTATION(#246,#10420) ;
#282 = CONTEXT_DEPENDENT_SHAPE_REPRESENTATION(#247,#10421) ;
#283 = CONTEXT_DEPENDENT_SHAPE_REPRESENTATION(#248,#10422) ;
#284 = CONTEXT_DEPENDENT_SHAPE_REPRESENTATION(#249,#10423) ;
#285 = CONTEXT_DEPENDENT_SHAPE_REPRESENTATION(#250,#10424) ;
#286 = CONTEXT_DEPENDENT_SHAPE_REPRESENTATION(#251,#10429) ;
#287 = CONTEXT_DEPENDENT_SHAPE_REPRESENTATION(#252,#10430) ;
#288 = CONTEXT_DEPENDENT_SHAPE_REPRESENTATION(#253,#10431) ;
#289 = CONTEXT_DEPENDENT_SHAPE_REPRESENTATION(#254,#10438) ;
#290 = CONTEXT_DEPENDENT_SHAPE_REPRESENTATION(#255,#10439) ;
#291 = CONTEXT_DEPENDENT_SHAPE_REPRESENTATION(#256,#10440) ;
#292 = CONTEXT_DEPENDENT_SHAPE_REPRESENTATION(#257,#10441) ;
#293 = CONTEXT_DEPENDENT_SHAPE_REPRESENTATION(#258,#10442) ;
#294 = CONTEXT_DEPENDENT_SHAPE_REPRESENTATION(#259,#10443) ;
#295 = CONTEXT_DEPENDENT_SHAPE_REPRESENTATION(#260,#10444) ;
#296 = CONTEXT_DEPENDENT_SHAPE_REPRESENTATION(#261,#10445) ;
#297 = NEXT_ASSEMBLY_USAGE_OCCURRENCE('Guard_Mounting_Ring_1:1',
'Guard_Mounting_Ring_1:1','Guard_Mounting_Ring_1:1',#10484,#10485,
'Guard_Mounting_Ring_1:1') ;
#298 = NEXT_ASSEMBLY_USAGE_OCCURRENCE('Guard_Mounting_Ring_2:1',
'Guard_Mounting_Ring_2:1','Guard_Mounting_Ring_2:1',#10484,#10486,
'Guard_Mounting_Ring_2:1') ;
#299 = NEXT_ASSEMBLY_USAGE_OCCURRENCE('Guard_Ring_1:1','Guard_Ring_1:1',
'Guard_Ring_1:1',#10484,#10487,'Guard_Ring_1:1') ;
#300 = NEXT_ASSEMBLY_USAGE_OCCURRENCE('Guard_Ring_2:1','Guard_Ring_2:1',
'Guard_Ring_2:1',#10484,#10488,'Guard_Ring_2:1') ;
#301 = NEXT_ASSEMBLY_USAGE_OCCURRENCE('Guard_Ring_3:1','Guard_Ring_3:1',
'Guard_Ring_3:1',#10484,#10489,'Guard_Ring_3:1') ;
#302 = NEXT_ASSEMBLY_USAGE_OCCURRENCE('Guard_Ring_4:1','Guard_Ring_4:1',
'Guard_Ring_4:1',#10484,#10490,'Guard_Ring_4:1') ;
#303 = NEXT_ASSEMBLY_USAGE_OCCURRENCE('Guard_Ring_5:1','Guard_Ring_5:1',
'Guard_Ring_5:1',#10484,#10491,'Guard_Ring_5:1') ;
#304 = NEXT_ASSEMBLY_USAGE_OCCURRENCE('Guard_Ring_6:1','Guard_Ring_6:1',
'Guard_Ring_6:1',#10484,#10492,'Guard_Ring_6:1') ;
#305 = NEXT_ASSEMBLY_USAGE_OCCURRENCE('Guard_Ring_7:1','Guard_Ring_7:1',
'Guard_Ring_7:1',#10484,#10493,'Guard_Ring_7:1') ;
#306 = NEXT_ASSEMBLY_USAGE_OCCURRENCE('Guard_Ring_8:1','Guard_Ring_8:1',
'Guard_Ring_8:1',#10484,#10494,'Guard_Ring_8:1') ;
#307 = NEXT_ASSEMBLY_USAGE_OCCURRENCE('Guard_Ring_9:1','Guard_Ring_9:1',
'Guard_Ring_9:1',#10484,#10495,'Guard_Ring_9:1') ;
#308 = NEXT_ASSEMBLY_USAGE_OCCURRENCE('Guard_Ring_10:1','Guard_Ring_10:1',
'Guard_Ring_10:1',#10484,#10496,'Guard_Ring_10:1') ;
#309 = NEXT_ASSEMBLY_USAGE_OCCURRENCE('Guard_Ring_11:1','Guard_Ring_11:1',
'Guard_Ring_11:1',#10484,#10497,'Guard_Ring_11:1') ;
#310 = NEXT_ASSEMBLY_USAGE_OCCURRENCE('Guard_Ring_12:1','Guard_Ring_12:1',
'Guard_Ring_12:1',#10484,#10498,'Guard_Ring_12:1') ;
#311 = NEXT_ASSEMBLY_USAGE_OCCURRENCE('Guard_Ring_13:1','Guard_Ring_13:1',
'Guard_Ring_13:1',#10484,#10499,'Guard_Ring_13:1') ;
#312 = NEXT_ASSEMBLY_USAGE_OCCURRENCE('Guard_Ring_14:1','Guard_Ring_14:1',
'Guard_Ring_14:1',#10484,#10500,'Guard_Ring_14:1') ;
#313 = NEXT_ASSEMBLY_USAGE_OCCURRENCE('Guard_Ring_15:1','Guard_Ring_15:1',
'Guard_Ring_15:1',#10484,#10501,'Guard_Ring_15:1') ;
#314 = NEXT_ASSEMBLY_USAGE_OCCURRENCE('Guard_Ring_16:1','Guard_Ring_16:1',
'Guard_Ring_16:1',#10484,#10502,'Guard_Ring_16:1') ;
#315 = NEXT_ASSEMBLY_USAGE_OCCURRENCE('Guard_Ring_17:1','Guard_Ring_17:1',
'Guard_Ring_17:1',#10484,#10503,'Guard_Ring_17:1') ;
#316 = NEXT_ASSEMBLY_USAGE_OCCURRENCE('Guard_Ring_18:1','Guard_Ring_18:1',
'Guard_Ring_18:1',#10484,#10504,'Guard_Ring_18:1') ;
#317 = NEXT_ASSEMBLY_USAGE_OCCURRENCE('Guard_Ring_19:1','Guard_Ring_19:1',
'Guard_Ring_19:1',#10484,#10505,'Guard_Ring_19:1') ;
#318 = NEXT_ASSEMBLY_USAGE_OCCURRENCE('Guard_Ring_20:1','Guard_Ring_20:1',
'Guard_Ring_20:1',#10484,#10506,'Guard_Ring_20:1') ;
#319 = NEXT_ASSEMBLY_USAGE_OCCURRENCE('Guard_Ring_21:1','Guard_Ring_21:1',
'Guard_Ring_21:1',#10484,#10507,'Guard_Ring_21:1') ;
#320 = NEXT_ASSEMBLY_USAGE_OCCURRENCE('Guard_Ring_22:1','Guard_Ring_22:1',
'Guard_Ring_22:1',#10484,#10508,'Guard_Ring_22:1') ;
#321 = NEXT_ASSEMBLY_USAGE_OCCURRENCE('Impeller:1','Impeller:1',
'Impeller:1',#10509,#10510,'Impeller:1') ;
#322 = NEXT_ASSEMBLY_USAGE_OCCURRENCE('Ring:1','Ring:1','Ring:1',#10509,#10511,
'Ring:1') ;
#323 = NEXT_ASSEMBLY_USAGE_OCCURRENCE('Motor:1','Motor:1','Motor:1',#10509,
#10512,'Motor:1') ;
#324 = NEXT_ASSEMBLY_USAGE_OCCURRENCE('Mounting_Panel:1',
'Mounting_Panel:1','Mounting_Panel:1',#10513,#10514,'Mounting_Panel:1') ;
#325 = NEXT_ASSEMBLY_USAGE_OCCURRENCE('Mounting_Bracket_1:1',
'Mounting_Bracket_1:1','Mounting_Bracket_1:1',#10513,#10515,
'Mounting_Bracket_1:1') ;
#326 = NEXT_ASSEMBLY_USAGE_OCCURRENCE('Mounting_Bracket_2:1',
'Mounting_Bracket_2:1','Mounting_Bracket_2:1',#10513,#10516,
'Mounting_Bracket_2:1') ;
#327 = NEXT_ASSEMBLY_USAGE_OCCURRENCE('Mounting_Bracket_3:1',
'Mounting_Bracket_3:1','Mounting_Bracket_3:1',#10513,#10517,
'Mounting_Bracket_3:1') ;
#328 = NEXT_ASSEMBLY_USAGE_OCCURRENCE('Mounting_Bracket_4:1',
'Mounting_Bracket_4:1','Mounting_Bracket_4:1',#10513,#10518,
'Mounting_Bracket_4:1') ;
#329 = NEXT_ASSEMBLY_USAGE_OCCURRENCE('Guard_Assembly:1',
'Guard_Assembly:1','Guard_Assembly:1',#10483,#10484,'Guard_Assembly:1') ;
#330 = NEXT_ASSEMBLY_USAGE_OCCURRENCE('Fan_Assembly:1','Fan_Assembly:1',
'Fan_Assembly:1',#10483,#10509,'Fan_Assembly:1') ;
#331 = NEXT_ASSEMBLY_USAGE_OCCURRENCE('Mounting_Assembly:1',
'Mounting_Assembly:1','Mounting_Assembly:1',#10483,#10513,
'Mounting_Assembly:1') ;
#332 = SHAPE_REPRESENTATION_RELATIONSHIP('SRR','None',#10448,#364) ;
#333 = SHAPE_REPRESENTATION_RELATIONSHIP('SRR','None',#10449,#365) ;
#334 = SHAPE_REPRESENTATION_RELATIONSHIP('SRR','None',#10450,#366) ;
#335 = SHAPE_REPRESENTATION_RELATIONSHIP('SRR','None',#10451,#367) ;
#336 = SHAPE_REPRESENTATION_RELATIONSHIP('SRR','None',#10452,#368) ;
#337 = SHAPE_REPRESENTATION_RELATIONSHIP('SRR','None',#10453,#369) ;
#338 = SHAPE_REPRESENTATION_RELATIONSHIP('SRR','None',#10454,#370) ;
#339 = SHAPE_REPRESENTATION_RELATIONSHIP('SRR','None',#10455,#371) ;
#340 = SHAPE_REPRESENTATION_RELATIONSHIP('SRR','None',#10456,#372) ;
#341 = SHAPE_REPRESENTATION_RELATIONSHIP('SRR','None',#10457,#373) ;
#342 = SHAPE_REPRESENTATION_RELATIONSHIP('SRR','None',#10458,#374) ;
#343 = SHAPE_REPRESENTATION_RELATIONSHIP('SRR','None',#10459,#375) ;
#344 = SHAPE_REPRESENTATION_RELATIONSHIP('SRR','None',#10460,#376) ;
#345 = SHAPE_REPRESENTATION_RELATIONSHIP('SRR','None',#10461,#377) ;
#346 = SHAPE_REPRESENTATION_RELATIONSHIP('SRR','None',#10462,#378) ;
#347 = SHAPE_REPRESENTATION_RELATIONSHIP('SRR','None',#10463,#379) ;
#348 = SHAPE_REPRESENTATION_RELATIONSHIP('SRR','None',#10464,#380) ;
#349 = SHAPE_REPRESENTATION_RELATIONSHIP('SRR','None',#10465,#381) ;
#350 = SHAPE_REPRESENTATION_RELATIONSHIP('SRR','None',#10466,#382) ;
#351 = SHAPE_REPRESENTATION_RELATIONSHIP('SRR','None',#10467,#383) ;
#352 = SHAPE_REPRESENTATION_RELATIONSHIP('SRR','None',#10468,#384) ;
#353 = SHAPE_REPRESENTATION_RELATIONSHIP('SRR','None',#10469,#385) ;
#354 = SHAPE_REPRESENTATION_RELATIONSHIP('SRR','None',#10470,#386) ;
#355 = SHAPE_REPRESENTATION_RELATIONSHIP('SRR','None',#10471,#387) ;
#356 = SHAPE_REPRESENTATION_RELATIONSHIP('SRR','None',#10473,#388) ;
#357 = SHAPE_REPRESENTATION_RELATIONSHIP('SRR','None',#10474,#389) ;
#358 = SHAPE_REPRESENTATION_RELATIONSHIP('SRR','None',#10475,#390) ;
#359 = SHAPE_REPRESENTATION_RELATIONSHIP('SRR','None',#10477,#391) ;
#360 = SHAPE_REPRESENTATION_RELATIONSHIP('SRR','None',#10478,#392) ;
#361 = SHAPE_REPRESENTATION_RELATIONSHIP('SRR','None',#10479,#393) ;
#362 = SHAPE_REPRESENTATION_RELATIONSHIP('SRR','None',#10480,#394) ;
#363 = SHAPE_REPRESENTATION_RELATIONSHIP('SRR','None',#10481,#395) ;
#364 = ADVANCED_BREP_SHAPE_REPRESENTATION('',(#436),#10300) ;
#365 = ADVANCED_BREP_SHAPE_REPRESENTATION('',(#437),#10301) ;
#366 = ADVANCED_BREP_SHAPE_REPRESENTATION('',(#438),#10302) ;
#367 = ADVANCED_BREP_SHAPE_REPRESENTATION('',(#439),#10303) ;
#368 = ADVANCED_BREP_SHAPE_REPRESENTATION('',(#440),#10304) ;
#369 = ADVANCED_BREP_SHAPE_REPRESENTATION('',(#441),#10305) ;
#370 = ADVANCED_BREP_SHAPE_REPRESENTATION('',(#442),#10306) ;
#371 = ADVANCED_BREP_SHAPE_REPRESENTATION('',(#443),#10307) ;
#372 = ADVANCED_BREP_SHAPE_REPRESENTATION('',(#444),#10308) ;
#373 = ADVANCED_BREP_SHAPE_REPRESENTATION('',(#445),#10309) ;
#374 = ADVANCED_BREP_SHAPE_REPRESENTATION('',(#446),#10310) ;
#375 = ADVANCED_BREP_SHAPE_REPRESENTATION('',(#447),#10311) ;
#376 = ADVANCED_BREP_SHAPE_REPRESENTATION('',(#448),#10312) ;
#377 = ADVANCED_BREP_SHAPE_REPRESENTATION('',(#449),#10313) ;
#378 = ADVANCED_BREP_SHAPE_REPRESENTATION('',(#450),#10314) ;
#379 = ADVANCED_BREP_SHAPE_REPRESENTATION('',(#451),#10315) ;
#380 = ADVANCED_BREP_SHAPE_REPRESENTATION('',(#452),#10316) ;
#381 = ADVANCED_BREP_SHAPE_REPRESENTATION('',(#453),#10317) ;
#382 = ADVANCED_BREP_SHAPE_REPRESENTATION('',(#454),#10318) ;
#383 = ADVANCED_BREP_SHAPE_REPRESENTATION('',(#455),#10319) ;
#384 = ADVANCED_BREP_SHAPE_REPRESENTATION('',(#456),#10320) ;
#385 = ADVANCED_BREP_SHAPE_REPRESENTATION('',(#457),#10321) ;
#386 = ADVANCED_BREP_SHAPE_REPRESENTATION('',(#458),#10322) ;
#387 = ADVANCED_BREP_SHAPE_REPRESENTATION('',(#459),#10323) ;
#388 = ADVANCED_BREP_SHAPE_REPRESENTATION('',(#460),#10325) ;
#389 = ADVANCED_BREP_SHAPE_REPRESENTATION('',(#461),#10326) ;
#390 = ADVANCED_BREP_SHAPE_REPRESENTATION('',(#462),#10327) ;
#391 = ADVANCED_BREP_SHAPE_REPRESENTATION('',(#463),#10329) ;
#392 = ADVANCED_BREP_SHAPE_REPRESENTATION('',(#464),#10330) ;
#393 = ADVANCED_BREP_SHAPE_REPRESENTATION('',(#465),#10331) ;
#394 = ADVANCED_BREP_SHAPE_REPRESENTATION('',(#466),#10332) ;
#395 = ADVANCED_BREP_SHAPE_REPRESENTATION('',(#467),#10333) ;
#396 = STYLED_ITEM('',(#10631),#436) ;
#397 = STYLED_ITEM('',(#10631),#437) ;
#398 = STYLED_ITEM('',(#10631),#438) ;
#399 = STYLED_ITEM('',(#10631),#439) ;
#400 = STYLED_ITEM('',(#10631),#440) ;
#401 = STYLED_ITEM('',(#10631),#441) ;
#402 = STYLED_ITEM('',(#10631),#442) ;
#403 = STYLED_ITEM('',(#10631),#443) ;
#404 = STYLED_ITEM('',(#10631),#444) ;
#405 = STYLED_ITEM('',(#10631),#3374) ;
#406 = STYLED_ITEM('',(#10632),#445) ;
#407 = STYLED_ITEM('',(#10631),#3375) ;
#408 = STYLED_ITEM('',(#10632),#446) ;
#409 = STYLED_ITEM('',(#10631),#3376) ;
#410 = STYLED_ITEM('',(#10632),#447) ;
#411 = STYLED_ITEM('',(#10631),#3377) ;
#412 = STYLED_ITEM('',(#10632),#448) ;
#413 = STYLED_ITEM('',(#10631),#3378) ;
#414 = STYLED_ITEM('',(#10632),#449) ;
#415 = STYLED_ITEM('',(#10631),#3379) ;
#416 = STYLED_ITEM('',(#10632),#450) ;
#417 = STYLED_ITEM('',(#10631),#3380) ;
#418 = STYLED_ITEM('',(#10632),#451) ;
#419 = STYLED_ITEM('',(#10631),#452) ;
#420 = STYLED_ITEM('',(#10631),#3382) ;
#421 = STYLED_ITEM('',(#10632),#453) ;
#422 = STYLED_ITEM('',(#10631),#454) ;
#423 = STYLED_ITEM('',(#10631),#455) ;
#424 = STYLED_ITEM('',(#10631),#456) ;
#425 = STYLED_ITEM('',(#10631),#457) ;
#426 = STYLED_ITEM('',(#10632),#458) ;
#427 = STYLED_ITEM('',(#10632),#459) ;
#428 = STYLED_ITEM('',(#10633),#460) ;
#429 = STYLED_ITEM('',(#10631),#461) ;
#430 = STYLED_ITEM('',(#10631),#462) ;
#431 = STYLED_ITEM('',(#10631),#463) ;
#432 = STYLED_ITEM('',(#10631),#464) ;
#433 = STYLED_ITEM('',(#10631),#465) ;
#434 = STYLED_ITEM('',(#10631),#466) ;
#435 = STYLED_ITEM('',(#10631),#467) ;
#436 = MANIFOLD_SOLID_BREP('Body1',#3558) ;
#437 = MANIFOLD_SOLID_BREP('Body1',#3559) ;
#438 = MANIFOLD_SOLID_BREP('Body1',#3560) ;
#439 = MANIFOLD_SOLID_BREP('Body1',#3561) ;
#440 = MANIFOLD_SOLID_BREP('Body1',#3562) ;
#441 = MANIFOLD_SOLID_BREP('Body1',#3563) ;
#442 = MANIFOLD_SOLID_BREP('Body1',#3564) ;
#443 = MANIFOLD_SOLID_BREP('Body1',#3565) ;
#444 = MANIFOLD_SOLID_BREP('Body1',#3566) ;
#445 = MANIFOLD_SOLID_BREP('Body1',#3567) ;
#446 = MANIFOLD_SOLID_BREP('Body1',#3568) ;
#447 = MANIFOLD_SOLID_BREP('Body1',#3569) ;
#448 = MANIFOLD_SOLID_BREP('Body1',#3570) ;
#449 = MANIFOLD_SOLID_BREP('Body1',#3571) ;
#450 = MANIFOLD_SOLID_BREP('Body1',#3572) ;
#451 = MANIFOLD_SOLID_BREP('Body1',#3573) ;
#452 = MANIFOLD_SOLID_BREP('Body1',#3574) ;
#453 = MANIFOLD_SOLID_BREP('Body1',#3575) ;
#454 = MANIFOLD_SOLID_BREP('Body1',#3576) ;
#455 = MANIFOLD_SOLID_BREP('Body1',#3577) ;
#456 = MANIFOLD_SOLID_BREP('Body1',#3578) ;
#457 = MANIFOLD_SOLID_BREP('Body1',#3579) ;
#458 = MANIFOLD_SOLID_BREP('Body1',#3580) ;
#459 = MANIFOLD_SOLID_BREP('Body1',#3581) ;
#460 = MANIFOLD_SOLID_BREP('Body1',#3582) ;
#461 = MANIFOLD_SOLID_BREP('Body1',#3583) ;
#462 = MANIFOLD_SOLID_BREP('Body1',#3584) ;
#463 = MANIFOLD_SOLID_BREP('Body1',#3585) ;
#464 = MANIFOLD_SOLID_BREP('Body1',#3586) ;
#465 = MANIFOLD_SOLID_BREP('Body1',#3587) ;
#466 = MANIFOLD_SOLID_BREP('Body1',#3588) ;
#467 = MANIFOLD_SOLID_BREP('Body1',#3589) ;
#468 = FACE_BOUND('',#1054,.T.) ;
#469 = FACE_BOUND('',#1082,.T.) ;
#470 = FACE_BOUND('',#1083,.T.) ;
#471 = FACE_BOUND('',#1084,.T.) ;
#472 = FACE_BOUND('',#1085,.T.) ;
#473 = FACE_BOUND('',#1136,.T.) ;
#474 = FACE_BOUND('',#1138,.T.) ;
#475 = FACE_BOUND('',#1151,.T.) ;
#476 = FACE_BOUND('',#1153,.T.) ;
#477 = PLANE('',#3957) ;
#478 = PLANE('',#4096) ;
#479 = PLANE('',#4103) ;
#480 = PLANE('',#4104) ;
#481 = PLANE('',#4105) ;
#482 = PLANE('',#4112) ;
#483 = PLANE('',#4113) ;
#484 = PLANE('',#4114) ;
#485 = PLANE('',#4121) ;
#486 = PLANE('',#4122) ;
#487 = PLANE('',#4129) ;
#488 = PLANE('',#4130) ;
#489 = PLANE('',#4137) ;
#490 = PLANE('',#4145) ;
#491 = PLANE('',#4146) ;
#492 = PLANE('',#4148) ;
#493 = PLANE('',#4149) ;
#494 = PLANE('',#4150) ;
#495 = PLANE('',#4151) ;
#496 = PLANE('',#4152) ;
#497 = PLANE('',#4157) ;
#498 = PLANE('',#4174) ;
#499 = PLANE('',#4175) ;
#500 = PLANE('',#4176) ;
#501 = PLANE('',#4177) ;
#502 = PLANE('',#4178) ;
#503 = PLANE('',#4179) ;
#504 = PLANE('',#4180) ;
#505 = PLANE('',#4183) ;
#506 = PLANE('',#4188) ;
#507 = PLANE('',#4189) ;
#508 = PLANE('',#4190) ;
#509 = PLANE('',#4191) ;
#510 = PLANE('',#4192) ;
#511 = PLANE('',#4193) ;
#512 = PLANE('',#4196) ;
#513 = PLANE('',#4201) ;
#514 = PLANE('',#4202) ;
#515 = PLANE('',#4203) ;
#516 = PLANE('',#4204) ;
#517 = PLANE('',#4205) ;
#518 = PLANE('',#4206) ;
#519 = PLANE('',#4209) ;
#520 = PLANE('',#4214) ;
#521 = PLANE('',#4215) ;
#522 = PLANE('',#4216) ;
#523 = PLANE('',#4217) ;
#524 = PLANE('',#4218) ;
#525 = PLANE('',#4219) ;
#526 = PLANE('',#4222) ;
#527 = PLANE('',#4227) ;
#528 = PLANE('',#4228) ;
#529 = PLANE('',#4229) ;
#530 = PLANE('',#4230) ;
#531 = PLANE('',#4231) ;
#532 = LINE('',#5624,#690) ;
#533 = LINE('',#5639,#691) ;
#534 = LINE('',#5650,#692) ;
#535 = LINE('',#5791,#693) ;
#536 = LINE('',#5800,#694) ;
#537 = LINE('',#5867,#695) ;
#538 = LINE('',#5958,#696) ;
#539 = LINE('',#6143,#697) ;
#540 = LINE('',#6275,#698) ;
#541 = LINE('',#6405,#699) ;
#542 = LINE('',#6474,#700) ;
#543 = LINE('',#6501,#701) ;
#544 = LINE('',#6872,#702) ;
#545 = LINE('',#6874,#703) ;
#546 = LINE('',#6876,#704) ;
#547 = LINE('',#7112,#705) ;
#548 = LINE('',#7139,#706) ;
#549 = LINE('',#7510,#707) ;
#550 = LINE('',#7512,#708) ;
#551 = LINE('',#7514,#709) ;
#552 = LINE('',#7750,#710) ;
#553 = LINE('',#7777,#711) ;
#554 = LINE('',#8148,#712) ;
#555 = LINE('',#8150,#713) ;
#556 = LINE('',#8152,#714) ;
#557 = LINE('',#8387,#715) ;
#558 = LINE('',#8414,#716) ;
#559 = LINE('',#8785,#717) ;
#560 = LINE('',#8787,#718) ;
#561 = LINE('',#8789,#719) ;
#562 = LINE('',#9024,#720) ;
#563 = LINE('',#9051,#721) ;
#564 = LINE('',#9422,#722) ;
#565 = LINE('',#9424,#723) ;
#566 = LINE('',#9426,#724) ;
#567 = LINE('',#9663,#725) ;
#568 = LINE('',#9669,#726) ;
#569 = LINE('',#9677,#727) ;
#570 = LINE('',#9679,#728) ;
#571 = LINE('',#9681,#729) ;
#572 = LINE('',#9682,#730) ;
#573 = LINE('',#9686,#731) ;
#574 = LINE('',#9688,#732) ;
#575 = LINE('',#9690,#733) ;
#576 = LINE('',#9691,#734) ;
#577 = LINE('',#9695,#735) ;
#578 = LINE('',#9697,#736) ;
#579 = LINE('',#9699,#737) ;
#580 = LINE('',#9700,#738) ;
#581 = LINE('',#9704,#739) ;
#582 = LINE('',#9706,#740) ;
#583 = LINE('',#9708,#741) ;
#584 = LINE('',#9709,#742) ;
#585 = LINE('',#9733,#743) ;
#586 = LINE('',#9738,#744) ;
#587 = LINE('',#9740,#745) ;
#588 = LINE('',#9742,#746) ;
#589 = LINE('',#9744,#747) ;
#590 = LINE('',#9746,#748) ;
#591 = LINE('',#9748,#749) ;
#592 = LINE('',#9750,#750) ;
#593 = LINE('',#9751,#751) ;
#594 = LINE('',#9755,#752) ;
#595 = LINE('',#9757,#753) ;
#596 = LINE('',#9759,#754) ;
#597 = LINE('',#9761,#755) ;
#598 = LINE('',#9763,#756) ;
#599 = LINE('',#9765,#757) ;
#600 = LINE('',#9767,#758) ;
#601 = LINE('',#9768,#759) ;
#602 = LINE('',#9770,#760) ;
#603 = LINE('',#9771,#761) ;
#604 = LINE('',#9773,#762) ;
#605 = LINE('',#9774,#763) ;
#606 = LINE('',#9776,#764) ;
#607 = LINE('',#9777,#765) ;
#608 = LINE('',#9779,#766) ;
#609 = LINE('',#9780,#767) ;
#610 = LINE('',#9784,#768) ;
#611 = LINE('',#9791,#769) ;
#612 = LINE('',#9794,#770) ;
#613 = LINE('',#9796,#771) ;
#614 = LINE('',#9799,#772) ;
#615 = LINE('',#9801,#773) ;
#616 = LINE('',#9802,#774) ;
#617 = LINE('',#9805,#775) ;
#618 = LINE('',#9807,#776) ;
#619 = LINE('',#9808,#777) ;
#620 = LINE('',#9810,#778) ;
#621 = LINE('',#9812,#779) ;
#622 = LINE('',#9817,#780) ;
#623 = LINE('',#9824,#781) ;
#624 = LINE('',#9827,#782) ;
#625 = LINE('',#9829,#783) ;
#626 = LINE('',#9832,#784) ;
#627 = LINE('',#9834,#785) ;
#628 = LINE('',#9835,#786) ;
#629 = LINE('',#9838,#787) ;
#630 = LINE('',#9840,#788) ;
#631 = LINE('',#9841,#789) ;
#632 = LINE('',#9843,#790) ;
#633 = LINE('',#9845,#791) ;
#634 = LINE('',#9850,#792) ;
#635 = LINE('',#9857,#793) ;
#636 = LINE('',#9860,#794) ;
#637 = LINE('',#9862,#795) ;
#638 = LINE('',#9865,#796) ;
#639 = LINE('',#9867,#797) ;
#640 = LINE('',#9868,#798) ;
#641 = LINE('',#9871,#799) ;
#642 = LINE('',#9873,#800) ;
#643 = LINE('',#9874,#801) ;
#644 = LINE('',#9876,#802) ;
#645 = LINE('',#9878,#803) ;
#646 = LINE('',#9883,#804) ;
#647 = LINE('',#9890,#805) ;
#648 = LINE('',#9893,#806) ;
#649 = LINE('',#9895,#807) ;
#650 = LINE('',#9898,#808) ;
#651 = LINE('',#9900,#809) ;
#652 = LINE('',#9901,#810) ;
#653 = LINE('',#9904,#811) ;
#654 = LINE('',#9906,#812) ;
#655 = LINE('',#9907,#813) ;
#656 = LINE('',#9909,#814) ;
#657 = LINE('',#9911,#815) ;
#658 = LINE('',#9983,#816) ;
#659 = LINE('',#9985,#817) ;
#660 = LINE('',#9987,#818) ;
#661 = LINE('',#9989,#819) ;
#662 = LINE('',#9991,#820) ;
#663 = LINE('',#9993,#821) ;
#664 = LINE('',#9995,#822) ;
#665 = LINE('',#9997,#823) ;
#666 = LINE('',#10068,#824) ;
#667 = LINE('',#10070,#825) ;
#668 = LINE('',#10072,#826) ;
#669 = LINE('',#10074,#827) ;
#670 = LINE('',#10076,#828) ;
#671 = LINE('',#10078,#829) ;
#672 = LINE('',#10080,#830) ;
#673 = LINE('',#10082,#831) ;
#674 = LINE('',#10153,#832) ;
#675 = LINE('',#10155,#833) ;
#676 = LINE('',#10157,#834) ;
#677 = LINE('',#10159,#835) ;
#678 = LINE('',#10161,#836) ;
#679 = LINE('',#10163,#837) ;
#680 = LINE('',#10165,#838) ;
#681 = LINE('',#10167,#839) ;
#682 = LINE('',#10238,#840) ;
#683 = LINE('',#10240,#841) ;
#684 = LINE('',#10242,#842) ;
#685 = LINE('',#10244,#843) ;
#686 = LINE('',#10246,#844) ;
#687 = LINE('',#10248,#845) ;
#688 = LINE('',#10250,#846) ;
#689 = LINE('',#10252,#847) ;
#690 = VECTOR('',#4472,36.8410607518303) ;
#691 = VECTOR('',#4491,41.0104872556709) ;
#692 = VECTOR('',#4506,36.984442871488) ;
#693 = VECTOR('',#4739,7.6) ;
#694 = VECTOR('',#4742,7.6) ;
#695 = VECTOR('',#4747,100.) ;
#696 = VECTOR('',#4748,100.) ;
#697 = VECTOR('',#4751,100.) ;
#698 = VECTOR('',#4754,100.) ;
#699 = VECTOR('',#4757,100.) ;
#700 = VECTOR('',#4762,1.) ;
#701 = VECTOR('',#4763,1.) ;
#702 = VECTOR('',#4772,100.) ;
#703 = VECTOR('',#4775,100.) ;
#704 = VECTOR('',#4778,100.) ;
#705 = VECTOR('',#4785,1.) ;
#706 = VECTOR('',#4786,1.) ;
#707 = VECTOR('',#4795,100.) ;
#708 = VECTOR('',#4798,100.) ;
#709 = VECTOR('',#4801,100.) ;
#710 = VECTOR('',#4808,1.) ;
#711 = VECTOR('',#4809,1.) ;
#712 = VECTOR('',#4818,100.) ;
#713 = VECTOR('',#4821,100.) ;
#714 = VECTOR('',#4824,100.) ;
#715 = VECTOR('',#4829,1.) ;
#716 = VECTOR('',#4830,1.) ;
#717 = VECTOR('',#4839,100.) ;
#718 = VECTOR('',#4842,100.) ;
#719 = VECTOR('',#4845,100.) ;
#720 = VECTOR('',#4850,1.) ;
#721 = VECTOR('',#4851,1.) ;
#722 = VECTOR('',#4860,100.) ;
#723 = VECTOR('',#4863,100.) ;
#724 = VECTOR('',#4866,100.) ;
#725 = VECTOR('',#4875,35.75) ;
#726 = VECTOR('',#4882,35.9) ;
#727 = VECTOR('',#4893,100.) ;
#728 = VECTOR('',#4894,100.) ;
#729 = VECTOR('',#4895,100.) ;
#730 = VECTOR('',#4896,100.) ;
#731 = VECTOR('',#4899,100.) ;
#732 = VECTOR('',#4900,100.) ;
#733 = VECTOR('',#4901,100.) ;
#734 = VECTOR('',#4902,100.) ;
#735 = VECTOR('',#4905,100.) ;
#736 = VECTOR('',#4906,100.) ;
#737 = VECTOR('',#4907,100.) ;
#738 = VECTOR('',#4908,100.) ;
#739 = VECTOR('',#4911,100.) ;
#740 = VECTOR('',#4912,100.) ;
#741 = VECTOR('',#4913,100.) ;
#742 = VECTOR('',#4914,100.) ;
#743 = VECTOR('',#4957,41.0104872556708) ;
#744 = VECTOR('',#4962,100.) ;
#745 = VECTOR('',#4963,100.) ;
#746 = VECTOR('',#4964,100.) ;
#747 = VECTOR('',#4965,100.) ;
#748 = VECTOR('',#4966,100.) ;
#749 = VECTOR('',#4967,99.9999999999999) ;
#750 = VECTOR('',#4968,100.) ;
#751 = VECTOR('',#4969,100.) ;
#752 = VECTOR('',#4972,100.) ;
#753 = VECTOR('',#4973,100.) ;
#754 = VECTOR('',#4974,100.) ;
#755 = VECTOR('',#4975,100.) ;
#756 = VECTOR('',#4976,100.) ;
#757 = VECTOR('',#4977,100.) ;
#758 = VECTOR('',#4978,100.) ;
#759 = VECTOR('',#4979,99.9999999999999) ;
#760 = VECTOR('',#4982,100.) ;
#761 = VECTOR('',#4983,100.) ;
#762 = VECTOR('',#4986,100.) ;
#763 = VECTOR('',#4987,100.) ;
#764 = VECTOR('',#4990,100.) ;
#765 = VECTOR('',#4991,100.) ;
#766 = VECTOR('',#4994,100.) ;
#767 = VECTOR('',#4995,100.) ;
#768 = VECTOR('',#4998,100.) ;
#769 = VECTOR('',#5007,100.) ;
#770 = VECTOR('',#5012,100.) ;
#771 = VECTOR('',#5015,100.) ;
#772 = VECTOR('',#5018,100.) ;
#773 = VECTOR('',#5019,100.) ;
#774 = VECTOR('',#5020,100.) ;
#775 = VECTOR('',#5023,100.) ;
#776 = VECTOR('',#5024,100.) ;
#777 = VECTOR('',#5025,100.) ;
#778 = VECTOR('',#5028,100.) ;
#779 = VECTOR('',#5031,100.) ;
#780 = VECTOR('',#5036,100.) ;
#781 = VECTOR('',#5045,100.) ;
#782 = VECTOR('',#5050,100.) ;
#783 = VECTOR('',#5053,100.) ;
#784 = VECTOR('',#5056,100.) ;
#785 = VECTOR('',#5057,100.) ;
#786 = VECTOR('',#5058,100.) ;
#787 = VECTOR('',#5061,100.) ;
#788 = VECTOR('',#5062,100.) ;
#789 = VECTOR('',#5063,100.) ;
#790 = VECTOR('',#5066,100.) ;
#791 = VECTOR('',#5069,100.) ;
#792 = VECTOR('',#5074,100.) ;
#793 = VECTOR('',#5083,100.) ;
#794 = VECTOR('',#5088,100.) ;
#795 = VECTOR('',#5091,100.) ;
#796 = VECTOR('',#5094,100.) ;
#797 = VECTOR('',#5095,100.) ;
#798 = VECTOR('',#5096,100.) ;
#799 = VECTOR('',#5099,100.) ;
#800 = VECTOR('',#5100,100.) ;
#801 = VECTOR('',#5101,100.) ;
#802 = VECTOR('',#5104,100.) ;
#803 = VECTOR('',#5107,100.) ;
#804 = VECTOR('',#5112,100.) ;
#805 = VECTOR('',#5121,100.) ;
#806 = VECTOR('',#5126,100.) ;
#807 = VECTOR('',#5129,100.) ;
#808 = VECTOR('',#5132,100.) ;
#809 = VECTOR('',#5133,100.) ;
#810 = VECTOR('',#5134,100.) ;
#811 = VECTOR('',#5137,100.) ;
#812 = VECTOR('',#5138,100.) ;
#813 = VECTOR('',#5139,100.) ;
#814 = VECTOR('',#5142,100.) ;
#815 = VECTOR('',#5145,100.) ;
#816 = VECTOR('',#5236,0.600000000000001) ;
#817 = VECTOR('',#5239,0.600000000000001) ;
#818 = VECTOR('',#5242,0.599999999999996) ;
#819 = VECTOR('',#5245,0.600000000000001) ;
#820 = VECTOR('',#5248,0.600000000000001) ;
#821 = VECTOR('',#5251,0.600000000000001) ;
#822 = VECTOR('',#5254,0.599999999999996) ;
#823 = VECTOR('',#5257,0.600000000000001) ;
#824 = VECTOR('',#5346,0.600000000000001) ;
#825 = VECTOR('',#5349,0.600000000000001) ;
#826 = VECTOR('',#5352,0.599999999999996) ;
#827 = VECTOR('',#5355,0.600000000000001) ;
#828 = VECTOR('',#5358,0.600000000000001) ;
#829 = VECTOR('',#5361,0.600000000000001) ;
#830 = VECTOR('',#5364,0.599999999999996) ;
#831 = VECTOR('',#5367,0.600000000000001) ;
#832 = VECTOR('',#5456,0.600000000000001) ;
#833 = VECTOR('',#5459,0.600000000000001) ;
#834 = VECTOR('',#5462,0.599999999999997) ;
#835 = VECTOR('',#5465,0.600000000000001) ;
#836 = VECTOR('',#5468,0.600000000000001) ;
#837 = VECTOR('',#5471,0.600000000000001) ;
#838 = VECTOR('',#5474,0.599999999999997) ;
#839 = VECTOR('',#5477,0.600000000000001) ;
#840 = VECTOR('',#5566,0.600000000000001) ;
#841 = VECTOR('',#5569,0.600000000000001) ;
#842 = VECTOR('',#5572,0.599999999999996) ;
#843 = VECTOR('',#5575,0.600000000000001) ;
#844 = VECTOR('',#5578,0.600000000000001) ;
#845 = VECTOR('',#5581,0.600000000000001) ;
#846 = VECTOR('',#5584,0.599999999999996) ;
#847 = VECTOR('',#5587,0.600000000000001) ;
#848 = CONICAL_SURFACE('',#3956,36.8410607518303,0.812867971023228) ;
#849 = CONICAL_SURFACE('',#3965,41.0104872556709,0.416359756197082) ;
#850 = CONICAL_SURFACE('',#3972,36.984442871488,0.81286797102658) ;
#851 = FACE_OUTER_BOUND('',#1050,.T.) ;
#852 = FACE_OUTER_BOUND('',#1051,.T.) ;
#853 = FACE_OUTER_BOUND('',#1052,.T.) ;
#854 = FACE_OUTER_BOUND('',#1053,.T.) ;
#855 = FACE_OUTER_BOUND('',#1055,.T.) ;
#856 = FACE_OUTER_BOUND('',#1056,.T.) ;
#857 = FACE_OUTER_BOUND('',#1057,.T.) ;
#858 = FACE_OUTER_BOUND('',#1058,.T.) ;
#859 = FACE_OUTER_BOUND('',#1059,.T.) ;
#860 = FACE_OUTER_BOUND('',#1060,.T.) ;
#861 = FACE_OUTER_BOUND('',#1061,.T.) ;
#862 = FACE_OUTER_BOUND('',#1062,.T.) ;
#863 = FACE_OUTER_BOUND('',#1063,.T.) ;
#864 = FACE_OUTER_BOUND('',#1064,.T.) ;
#865 = FACE_OUTER_BOUND('',#1065,.T.) ;
#866 = FACE_OUTER_BOUND('',#1066,.T.) ;
#867 = FACE_OUTER_BOUND('',#1067,.T.) ;
#868 = FACE_OUTER_BOUND('',#1068,.T.) ;
#869 = FACE_OUTER_BOUND('',#1069,.T.) ;
#870 = FACE_OUTER_BOUND('',#1070,.T.) ;
#871 = FACE_OUTER_BOUND('',#1071,.T.) ;
#872 = FACE_OUTER_BOUND('',#1072,.T.) ;
#873 = FACE_OUTER_BOUND('',#1073,.T.) ;
#874 = FACE_OUTER_BOUND('',#1074,.T.) ;
#875 = FACE_OUTER_BOUND('',#1075,.T.) ;
#876 = FACE_OUTER_BOUND('',#1076,.T.) ;
#877 = FACE_OUTER_BOUND('',#1077,.T.) ;
#878 = FACE_OUTER_BOUND('',#1078,.T.) ;
#879 = FACE_OUTER_BOUND('',#1079,.T.) ;
#880 = FACE_OUTER_BOUND('',#1080,.T.) ;
#881 = FACE_OUTER_BOUND('',#1081,.T.) ;
#882 = FACE_OUTER_BOUND('',#1086,.T.) ;
#883 = FACE_OUTER_BOUND('',#1087,.T.) ;
#884 = FACE_OUTER_BOUND('',#1088,.T.) ;
#885 = FACE_OUTER_BOUND('',#1089,.T.) ;
#886 = FACE_OUTER_BOUND('',#1090,.T.) ;
#887 = FACE_OUTER_BOUND('',#1091,.T.) ;
#888 = FACE_OUTER_BOUND('',#1092,.T.) ;
#889 = FACE_OUTER_BOUND('',#1093,.T.) ;
#890 = FACE_OUTER_BOUND('',#1094,.T.) ;
#891 = FACE_OUTER_BOUND('',#1095,.T.) ;
#892 = FACE_OUTER_BOUND('',#1096,.T.) ;
#893 = FACE_OUTER_BOUND('',#1097,.T.) ;
#894 = FACE_OUTER_BOUND('',#1098,.T.) ;
#895 = FACE_OUTER_BOUND('',#1099,.T.) ;
#896 = FACE_OUTER_BOUND('',#1100,.T.) ;
#897 = FACE_OUTER_BOUND('',#1101,.T.) ;
#898 = FACE_OUTER_BOUND('',#1102,.T.) ;
#899 = FACE_OUTER_BOUND('',#1103,.T.) ;
#900 = FACE_OUTER_BOUND('',#1104,.T.) ;
#901 = FACE_OUTER_BOUND('',#1105,.T.) ;
#902 = FACE_OUTER_BOUND('',#1106,.T.) ;
#903 = FACE_OUTER_BOUND('',#1107,.T.) ;
#904 = FACE_OUTER_BOUND('',#1108,.T.) ;
#905 = FACE_OUTER_BOUND('',#1109,.T.) ;
#906 = FACE_OUTER_BOUND('',#1110,.T.) ;
#907 = FACE_OUTER_BOUND('',#1111,.T.) ;
#908 = FACE_OUTER_BOUND('',#1112,.T.) ;
#909 = FACE_OUTER_BOUND('',#1113,.T.) ;
#910 = FACE_OUTER_BOUND('',#1114,.T.) ;
#911 = FACE_OUTER_BOUND('',#1115,.T.) ;
#912 = FACE_OUTER_BOUND('',#1116,.T.) ;
#913 = FACE_OUTER_BOUND('',#1117,.T.) ;
#914 = FACE_OUTER_BOUND('',#1118,.T.) ;
#915 = FACE_OUTER_BOUND('',#1119,.T.) ;
#916 = FACE_OUTER_BOUND('',#1120,.T.) ;
#917 = FACE_OUTER_BOUND('',#1121,.T.) ;
#918 = FACE_OUTER_BOUND('',#1122,.T.) ;
#919 = FACE_OUTER_BOUND('',#1123,.T.) ;
#920 = FACE_OUTER_BOUND('',#1124,.T.) ;
#921 = FACE_OUTER_BOUND('',#1125,.T.) ;
#922 = FACE_OUTER_BOUND('',#1126,.T.) ;
#923 = FACE_OUTER_BOUND('',#1127,.T.) ;
#924 = FACE_OUTER_BOUND('',#1128,.T.) ;
#925 = FACE_OUTER_BOUND('',#1129,.T.) ;
#926 = FACE_OUTER_BOUND('',#1130,.T.) ;
#927 = FACE_OUTER_BOUND('',#1131,.T.) ;
#928 = FACE_OUTER_BOUND('',#1132,.T.) ;
#929 = FACE_OUTER_BOUND('',#1133,.T.) ;
#930 = FACE_OUTER_BOUND('',#1134,.T.) ;
#931 = FACE_OUTER_BOUND('',#1135,.T.) ;
#932 = FACE_OUTER_BOUND('',#1137,.T.) ;
#933 = FACE_OUTER_BOUND('',#1139,.T.) ;
#934 = FACE_OUTER_BOUND('',#1140,.T.) ;
#935 = FACE_OUTER_BOUND('',#1141,.T.) ;
#936 = FACE_OUTER_BOUND('',#1142,.T.) ;
#937 = FACE_OUTER_BOUND('',#1143,.T.) ;
#938 = FACE_OUTER_BOUND('',#1144,.T.) ;
#939 = FACE_OUTER_BOUND('',#1145,.T.) ;
#940 = FACE_OUTER_BOUND('',#1146,.T.) ;
#941 = FACE_OUTER_BOUND('',#1147,.T.) ;
#942 = FACE_OUTER_BOUND('',#1148,.T.) ;
#943 = FACE_OUTER_BOUND('',#1149,.T.) ;
#944 = FACE_OUTER_BOUND('',#1150,.T.) ;
#945 = FACE_OUTER_BOUND('',#1152,.T.) ;
#946 = FACE_OUTER_BOUND('',#1154,.T.) ;
#947 = FACE_OUTER_BOUND('',#1155,.T.) ;
#948 = FACE_OUTER_BOUND('',#1156,.T.) ;
#949 = FACE_OUTER_BOUND('',#1157,.T.) ;
#950 = FACE_OUTER_BOUND('',#1158,.T.) ;
#951 = FACE_OUTER_BOUND('',#1159,.T.) ;
#952 = FACE_OUTER_BOUND('',#1160,.T.) ;
#953 = FACE_OUTER_BOUND('',#1161,.T.) ;
#954 = FACE_OUTER_BOUND('',#1162,.T.) ;
#955 = FACE_OUTER_BOUND('',#1163,.T.) ;
#956 = FACE_OUTER_BOUND('',#1164,.T.) ;
#957 = FACE_OUTER_BOUND('',#1165,.T.) ;
#958 = FACE_OUTER_BOUND('',#1166,.T.) ;
#959 = FACE_OUTER_BOUND('',#1167,.T.) ;
#960 = FACE_OUTER_BOUND('',#1168,.T.) ;
#961 = FACE_OUTER_BOUND('',#1169,.T.) ;
#962 = FACE_OUTER_BOUND('',#1170,.T.) ;
#963 = FACE_OUTER_BOUND('',#1171,.T.) ;
#964 = FACE_OUTER_BOUND('',#1172,.T.) ;
#965 = FACE_OUTER_BOUND('',#1173,.T.) ;
#966 = FACE_OUTER_BOUND('',#1174,.T.) ;
#967 = FACE_OUTER_BOUND('',#1175,.T.) ;
#968 = FACE_OUTER_BOUND('',#1176,.T.) ;
#969 = FACE_OUTER_BOUND('',#1177,.T.) ;
#970 = FACE_OUTER_BOUND('',#1178,.T.) ;
#971 = FACE_OUTER_BOUND('',#1179,.T.) ;
#972 = FACE_OUTER_BOUND('',#1180,.T.) ;
#973 = FACE_OUTER_BOUND('',#1181,.T.) ;
#974 = FACE_OUTER_BOUND('',#1182,.T.) ;
#975 = FACE_OUTER_BOUND('',#1183,.T.) ;
#976 = FACE_OUTER_BOUND('',#1184,.T.) ;
#977 = FACE_OUTER_BOUND('',#1185,.T.) ;
#978 = FACE_OUTER_BOUND('',#1186,.T.) ;
#979 = FACE_OUTER_BOUND('',#1187,.T.) ;
#980 = FACE_OUTER_BOUND('',#1188,.T.) ;
#981 = FACE_OUTER_BOUND('',#1189,.T.) ;
#982 = FACE_OUTER_BOUND('',#1190,.T.) ;
#983 = FACE_OUTER_BOUND('',#1191,.T.) ;
#984 = FACE_OUTER_BOUND('',#1192,.T.) ;
#985 = FACE_OUTER_BOUND('',#1193,.T.) ;
#986 = FACE_OUTER_BOUND('',#1194,.T.) ;
#987 = FACE_OUTER_BOUND('',#1195,.T.) ;
#988 = FACE_OUTER_BOUND('',#1196,.T.) ;
#989 = FACE_OUTER_BOUND('',#1197,.T.) ;
#990 = FACE_OUTER_BOUND('',#1198,.T.) ;
#991 = FACE_OUTER_BOUND('',#1199,.T.) ;
#992 = FACE_OUTER_BOUND('',#1200,.T.) ;
#993 = FACE_OUTER_BOUND('',#1201,.T.) ;
#994 = FACE_OUTER_BOUND('',#1202,.T.) ;
#995 = FACE_OUTER_BOUND('',#1203,.T.) ;
#996 = FACE_OUTER_BOUND('',#1204,.T.) ;
#997 = FACE_OUTER_BOUND('',#1205,.T.) ;
#998 = FACE_OUTER_BOUND('',#1206,.T.) ;
#999 = FACE_OUTER_BOUND('',#1207,.T.) ;
#1000 = FACE_OUTER_BOUND('',#1208,.T.) ;
#1001 = FACE_OUTER_BOUND('',#1209,.T.) ;
#1002 = FACE_OUTER_BOUND('',#1210,.T.) ;
#1003 = FACE_OUTER_BOUND('',#1211,.T.) ;
#1004 = FACE_OUTER_BOUND('',#1212,.T.) ;
#1005 = FACE_OUTER_BOUND('',#1213,.T.) ;
#1006 = FACE_OUTER_BOUND('',#1214,.T.) ;
#1007 = FACE_OUTER_BOUND('',#1215,.T.) ;
#1008 = FACE_OUTER_BOUND('',#1216,.T.) ;
#1009 = FACE_OUTER_BOUND('',#1217,.T.) ;
#1010 = FACE_OUTER_BOUND('',#1218,.T.) ;
#1011 = FACE_OUTER_BOUND('',#1219,.T.) ;
#1012 = FACE_OUTER_BOUND('',#1220,.T.) ;
#1013 = FACE_OUTER_BOUND('',#1221,.T.) ;
#1014 = FACE_OUTER_BOUND('',#1222,.T.) ;
#1015 = FACE_OUTER_BOUND('',#1223,.T.) ;
#1016 = FACE_OUTER_BOUND('',#1224,.T.) ;
#1017 = FACE_OUTER_BOUND('',#1225,.T.) ;
#1018 = FACE_OUTER_BOUND('',#1226,.T.) ;
#1019 = FACE_OUTER_BOUND('',#1227,.T.) ;
#1020 = FACE_OUTER_BOUND('',#1228,.T.) ;
#1021 = FACE_OUTER_BOUND('',#1229,.T.) ;
#1022 = FACE_OUTER_BOUND('',#1230,.T.) ;
#1023 = FACE_OUTER_BOUND('',#1231,.T.) ;
#1024 = FACE_OUTER_BOUND('',#1232,.T.) ;
#1025 = FACE_OUTER_BOUND('',#1233,.T.) ;
#1026 = FACE_OUTER_BOUND('',#1234,.T.) ;
#1027 = FACE_OUTER_BOUND('',#1235,.T.) ;
#1028 = FACE_OUTER_BOUND('',#1236,.T.) ;
#1029 = FACE_OUTER_BOUND('',#1237,.T.) ;
#1030 = FACE_OUTER_BOUND('',#1238,.T.) ;
#1031 = FACE_OUTER_BOUND('',#1239,.T.) ;
#1032 = FACE_OUTER_BOUND('',#1240,.T.) ;
#1033 = FACE_OUTER_BOUND('',#1241,.T.) ;
#1034 = FACE_OUTER_BOUND('',#1242,.T.) ;
#1035 = FACE_OUTER_BOUND('',#1243,.T.) ;
#1036 = FACE_OUTER_BOUND('',#1244,.T.) ;
#1037 = FACE_OUTER_BOUND('',#1245,.T.) ;
#1038 = FACE_OUTER_BOUND('',#1246,.T.) ;
#1039 = FACE_OUTER_BOUND('',#1247,.T.) ;
#1040 = FACE_OUTER_BOUND('',#1248,.T.) ;
#1041 = FACE_OUTER_BOUND('',#1249,.T.) ;
#1042 = FACE_OUTER_BOUND('',#1250,.T.) ;
#1043 = FACE_OUTER_BOUND('',#1251,.T.) ;
#1044 = FACE_OUTER_BOUND('',#1252,.T.) ;
#1045 = FACE_OUTER_BOUND('',#1253,.T.) ;
#1046 = FACE_OUTER_BOUND('',#1254,.T.) ;
#1047 = FACE_OUTER_BOUND('',#1255,.T.) ;
#1048 = FACE_OUTER_BOUND('',#1256,.T.) ;
#1049 = FACE_OUTER_BOUND('',#1257,.T.) ;
#1050 = EDGE_LOOP('',(#2307,#2308,#2309,#2310,#2311)) ;
#1051 = EDGE_LOOP('',(#2312,#2313,#2314,#2315,#2316)) ;
#1052 = EDGE_LOOP('',(#2317,#2318,#2319,#2320,#2321,#2322)) ;
#1053 = EDGE_LOOP('',(#2323)) ;
#1054 = EDGE_LOOP('',(#2324)) ;
#1055 = EDGE_LOOP('',(#2325,#2326,#2327,#2328,#2329,#2330)) ;
#1056 = EDGE_LOOP('',(#2331,#2332,#2333,#2334,#2335,#2336)) ;
#1057 = EDGE_LOOP('',(#2337,#2338,#2339,#2340,#2341,#2342)) ;
#1058 = EDGE_LOOP('',(#2343,#2344,#2345,#2346,#2347,#2348)) ;
#1059 = EDGE_LOOP('',(#2349,#2350,#2351,#2352)) ;
#1060 = EDGE_LOOP('',(#2353,#2354,#2355,#2356)) ;
#1061 = EDGE_LOOP('',(#2357,#2358,#2359,#2360)) ;
#1062 = EDGE_LOOP('',(#2361,#2362,#2363,#2364)) ;
#1063 = EDGE_LOOP('',(#2365,#2366,#2367,#2368)) ;
#1064 = EDGE_LOOP('',(#2369,#2370,#2371,#2372)) ;
#1065 = EDGE_LOOP('',(#2373,#2374,#2375,#2376)) ;
#1066 = EDGE_LOOP('',(#2377,#2378,#2379,#2380)) ;
#1067 = EDGE_LOOP('',(#2381,#2382,#2383,#2384)) ;
#1068 = EDGE_LOOP('',(#2385,#2386,#2387,#2388)) ;
#1069 = EDGE_LOOP('',(#2389,#2390,#2391,#2392)) ;
#1070 = EDGE_LOOP('',(#2393,#2394,#2395,#2396)) ;
#1071 = EDGE_LOOP('',(#2397,#2398,#2399,#2400)) ;
#1072 = EDGE_LOOP('',(#2401,#2402,#2403,#2404)) ;
#1073 = EDGE_LOOP('',(#2405,#2406,#2407,#2408)) ;
#1074 = EDGE_LOOP('',(#2409,#2410,#2411,#2412)) ;
#1075 = EDGE_LOOP('',(#2413,#2414,#2415,#2416)) ;
#1076 = EDGE_LOOP('',(#2417,#2418,#2419,#2420)) ;
#1077 = EDGE_LOOP('',(#2421,#2422,#2423,#2424)) ;
#1078 = EDGE_LOOP('',(#2425,#2426,#2427,#2428)) ;
#1079 = EDGE_LOOP('',(#2429,#2430,#2431,#2432)) ;
#1080 = EDGE_LOOP('',(#2433,#2434,#2435,#2436)) ;
#1081 = EDGE_LOOP('',(#2437,#2438,#2439,#2440,#2441,#2442,#2443,#2444,#2445,
#2446,#2447,#2448,#2449)) ;
#1082 = EDGE_LOOP('',(#2450,#2451,#2452,#2453,#2454,#2455,#2456)) ;
#1083 = EDGE_LOOP('',(#2457,#2458,#2459,#2460,#2461)) ;
#1084 = EDGE_LOOP('',(#2462,#2463,#2464,#2465,#2466)) ;
#1085 = EDGE_LOOP('',(#2467,#2468,#2469,#2470,#2471)) ;
#1086 = EDGE_LOOP('',(#2472,#2473,#2474,#2475,#2476,#2477,#2478)) ;
#1087 = EDGE_LOOP('',(#2479,#2480,#2481,#2482,#2483,#2484,#2485,#2486)) ;
#1088 = EDGE_LOOP('',(#2487,#2488,#2489,#2490,#2491,#2492)) ;
#1089 = EDGE_LOOP('',(#2493,#2494,#2495,#2496,#2497)) ;
#1090 = EDGE_LOOP('',(#2498,#2499,#2500,#2501)) ;
#1091 = EDGE_LOOP('',(#2502,#2503,#2504,#2505,#2506)) ;
#1092 = EDGE_LOOP('',(#2507,#2508,#2509,#2510,#2511,#2512)) ;
#1093 = EDGE_LOOP('',(#2513)) ;
#1094 = EDGE_LOOP('',(#2514,#2515,#2516,#2517,#2518)) ;
#1095 = EDGE_LOOP('',(#2519,#2520,#2521,#2522,#2523)) ;
#1096 = EDGE_LOOP('',(#2524,#2525,#2526,#2527,#2528,#2529)) ;
#1097 = EDGE_LOOP('',(#2530,#2531,#2532,#2533,#2534,#2535,#2536,#2537)) ;
#1098 = EDGE_LOOP('',(#2538,#2539,#2540,#2541,#2542,#2543)) ;
#1099 = EDGE_LOOP('',(#2544,#2545,#2546,#2547,#2548)) ;
#1100 = EDGE_LOOP('',(#2549,#2550,#2551,#2552)) ;
#1101 = EDGE_LOOP('',(#2553,#2554,#2555,#2556,#2557)) ;
#1102 = EDGE_LOOP('',(#2558,#2559,#2560,#2561,#2562,#2563)) ;
#1103 = EDGE_LOOP('',(#2564,#2565,#2566,#2567,#2568)) ;
#1104 = EDGE_LOOP('',(#2569,#2570,#2571,#2572)) ;
#1105 = EDGE_LOOP('',(#2573)) ;
#1106 = EDGE_LOOP('',(#2574,#2575,#2576,#2577,#2578,#2579)) ;
#1107 = EDGE_LOOP('',(#2580,#2581,#2582,#2583,#2584,#2585,#2586,#2587)) ;
#1108 = EDGE_LOOP('',(#2588,#2589,#2590,#2591,#2592,#2593)) ;
#1109 = EDGE_LOOP('',(#2594,#2595,#2596,#2597,#2598)) ;
#1110 = EDGE_LOOP('',(#2599,#2600,#2601,#2602)) ;
#1111 = EDGE_LOOP('',(#2603,#2604,#2605,#2606,#2607)) ;
#1112 = EDGE_LOOP('',(#2608,#2609,#2610,#2611,#2612,#2613)) ;
#1113 = EDGE_LOOP('',(#2614,#2615,#2616,#2617,#2618)) ;
#1114 = EDGE_LOOP('',(#2619,#2620,#2621,#2622)) ;
#1115 = EDGE_LOOP('',(#2623,#2624,#2625,#2626,#2627,#2628)) ;
#1116 = EDGE_LOOP('',(#2629,#2630,#2631,#2632,#2633,#2634,#2635,#2636)) ;
#1117 = EDGE_LOOP('',(#2637,#2638,#2639,#2640,#2641,#2642)) ;
#1118 = EDGE_LOOP('',(#2643,#2644,#2645,#2646,#2647)) ;
#1119 = EDGE_LOOP('',(#2648,#2649,#2650,#2651)) ;
#1120 = EDGE_LOOP('',(#2652,#2653,#2654,#2655,#2656)) ;
#1121 = EDGE_LOOP('',(#2657,#2658,#2659,#2660,#2661,#2662)) ;
#1122 = EDGE_LOOP('',(#2663,#2664,#2665,#2666,#2667,#2668)) ;
#1123 = EDGE_LOOP('',(#2669,#2670,#2671,#2672,#2673)) ;
#1124 = EDGE_LOOP('',(#2674,#2675,#2676,#2677,#2678,#2679)) ;
#1125 = EDGE_LOOP('',(#2680,#2681,#2682,#2683,#2684,#2685,#2686,#2687)) ;
#1126 = EDGE_LOOP('',(#2688,#2689,#2690,#2691,#2692,#2693)) ;
#1127 = EDGE_LOOP('',(#2694,#2695,#2696,#2697,#2698)) ;
#1128 = EDGE_LOOP('',(#2699,#2700,#2701,#2702)) ;
#1129 = EDGE_LOOP('',(#2703,#2704,#2705,#2706,#2707)) ;
#1130 = EDGE_LOOP('',(#2708,#2709,#2710,#2711,#2712,#2713)) ;
#1131 = EDGE_LOOP('',(#2714,#2715,#2716,#2717,#2718)) ;
#1132 = EDGE_LOOP('',(#2719,#2720,#2721,#2722)) ;
#1133 = EDGE_LOOP('',(#2723,#2724,#2725,#2726)) ;
#1134 = EDGE_LOOP('',(#2727,#2728,#2729,#2730)) ;
#1135 = EDGE_LOOP('',(#2731)) ;
#1136 = EDGE_LOOP('',(#2732)) ;
#1137 = EDGE_LOOP('',(#2733)) ;
#1138 = EDGE_LOOP('',(#2734)) ;
#1139 = EDGE_LOOP('',(#2735,#2736,#2737,#2738)) ;
#1140 = EDGE_LOOP('',(#2739,#2740,#2741,#2742)) ;
#1141 = EDGE_LOOP('',(#2743,#2744,#2745,#2746)) ;
#1142 = EDGE_LOOP('',(#2747,#2748,#2749,#2750)) ;
#1143 = EDGE_LOOP('',(#2751,#2752,#2753,#2754,#2755,#2756,#2757,#2758)) ;
#1144 = EDGE_LOOP('',(#2759,#2760,#2761,#2762,#2763,#2764,#2765,#2766)) ;
#1145 = EDGE_LOOP('',(#2767,#2768,#2769,#2770)) ;
#1146 = EDGE_LOOP('',(#2771,#2772,#2773,#2774)) ;
#1147 = EDGE_LOOP('',(#2775,#2776,#2777,#2778)) ;
#1148 = EDGE_LOOP('',(#2779,#2780,#2781,#2782)) ;
#1149 = EDGE_LOOP('',(#2783,#2784,#2785,#2786)) ;
#1150 = EDGE_LOOP('',(#2787,#2788,#2789,#2790,#2791,#2792,#2793,#2794)) ;
#1151 = EDGE_LOOP('',(#2795)) ;
#1152 = EDGE_LOOP('',(#2796,#2797,#2798,#2799,#2800,#2801,#2802,#2803)) ;
#1153 = EDGE_LOOP('',(#2804)) ;
#1154 = EDGE_LOOP('',(#2805,#2806,#2807,#2808)) ;
#1155 = EDGE_LOOP('',(#2809,#2810,#2811,#2812)) ;
#1156 = EDGE_LOOP('',(#2813,#2814,#2815,#2816)) ;
#1157 = EDGE_LOOP('',(#2817,#2818,#2819,#2820)) ;
#1158 = EDGE_LOOP('',(#2821,#2822,#2823,#2824)) ;
#1159 = EDGE_LOOP('',(#2825,#2826,#2827,#2828)) ;
#1160 = EDGE_LOOP('',(#2829,#2830,#2831,#2832)) ;
#1161 = EDGE_LOOP('',(#2833,#2834,#2835,#2836)) ;
#1162 = EDGE_LOOP('',(#2837,#2838,#2839,#2840)) ;
#1163 = EDGE_LOOP('',(#2841,#2842,#2843,#2844)) ;
#1164 = EDGE_LOOP('',(#2845,#2846,#2847,#2848)) ;
#1165 = EDGE_LOOP('',(#2849,#2850,#2851,#2852)) ;
#1166 = EDGE_LOOP('',(#2853,#2854,#2855,#2856)) ;
#1167 = EDGE_LOOP('',(#2857,#2858,#2859,#2860)) ;
#1168 = EDGE_LOOP('',(#2861,#2862,#2863,#2864)) ;
#1169 = EDGE_LOOP('',(#2865,#2866,#2867,#2868)) ;
#1170 = EDGE_LOOP('',(#2869,#2870,#2871,#2872)) ;
#1171 = EDGE_LOOP('',(#2873,#2874,#2875,#2876)) ;
#1172 = EDGE_LOOP('',(#2877,#2878,#2879,#2880)) ;
#1173 = EDGE_LOOP('',(#2881,#2882,#2883,#2884)) ;
#1174 = EDGE_LOOP('',(#2885,#2886,#2887,#2888)) ;
#1175 = EDGE_LOOP('',(#2889,#2890,#2891,#2892)) ;
#1176 = EDGE_LOOP('',(#2893,#2894,#2895,#2896)) ;
#1177 = EDGE_LOOP('',(#2897,#2898,#2899,#2900)) ;
#1178 = EDGE_LOOP('',(#2901,#2902,#2903,#2904)) ;
#1179 = EDGE_LOOP('',(#2905,#2906,#2907,#2908)) ;
#1180 = EDGE_LOOP('',(#2909,#2910,#2911,#2912)) ;
#1181 = EDGE_LOOP('',(#2913,#2914,#2915,#2916)) ;
#1182 = EDGE_LOOP('',(#2917,#2918,#2919,#2920)) ;
#1183 = EDGE_LOOP('',(#2921,#2922,#2923,#2924)) ;
#1184 = EDGE_LOOP('',(#2925,#2926,#2927,#2928)) ;
#1185 = EDGE_LOOP('',(#2929,#2930,#2931,#2932)) ;
#1186 = EDGE_LOOP('',(#2933,#2934,#2935,#2936)) ;
#1187 = EDGE_LOOP('',(#2937,#2938,#2939,#2940)) ;
#1188 = EDGE_LOOP('',(#2941,#2942,#2943,#2944)) ;
#1189 = EDGE_LOOP('',(#2945,#2946,#2947,#2948)) ;
#1190 = EDGE_LOOP('',(#2949,#2950,#2951,#2952)) ;
#1191 = EDGE_LOOP('',(#2953,#2954,#2955,#2956)) ;
#1192 = EDGE_LOOP('',(#2957,#2958,#2959,#2960)) ;
#1193 = EDGE_LOOP('',(#2961,#2962,#2963,#2964)) ;
#1194 = EDGE_LOOP('',(#2965,#2966,#2967,#2968,#2969)) ;
#1195 = EDGE_LOOP('',(#2970,#2971,#2972,#2973)) ;
#1196 = EDGE_LOOP('',(#2974,#2975,#2976,#2977,#2978,#2979)) ;
#1197 = EDGE_LOOP('',(#2980,#2981,#2982,#2983,#2984,#2985)) ;
#1198 = EDGE_LOOP('',(#2986,#2987,#2988,#2989,#2990,#2991)) ;
#1199 = EDGE_LOOP('',(#2992,#2993,#2994,#2995,#2996)) ;
#1200 = EDGE_LOOP('',(#2997,#2998,#2999,#3000)) ;
#1201 = EDGE_LOOP('',(#3001,#3002,#3003,#3004,#3005,#3006)) ;
#1202 = EDGE_LOOP('',(#3007,#3008,#3009,#3010,#3011,#3012)) ;
#1203 = EDGE_LOOP('',(#3013,#3014,#3015,#3016)) ;
#1204 = EDGE_LOOP('',(#3017,#3018,#3019,#3020,#3021)) ;
#1205 = EDGE_LOOP('',(#3022,#3023,#3024,#3025,#3026,#3027)) ;
#1206 = EDGE_LOOP('',(#3028,#3029,#3030,#3031,#3032,#3033)) ;
#1207 = EDGE_LOOP('',(#3034,#3035,#3036,#3037)) ;
#1208 = EDGE_LOOP('',(#3038,#3039,#3040,#3041,#3042)) ;
#1209 = EDGE_LOOP('',(#3043,#3044,#3045,#3046,#3047,#3048)) ;
#1210 = EDGE_LOOP('',(#3049,#3050,#3051,#3052,#3053)) ;
#1211 = EDGE_LOOP('',(#3054,#3055,#3056,#3057)) ;
#1212 = EDGE_LOOP('',(#3058,#3059,#3060,#3061,#3062,#3063)) ;
#1213 = EDGE_LOOP('',(#3064,#3065,#3066,#3067,#3068,#3069)) ;
#1214 = EDGE_LOOP('',(#3070,#3071,#3072,#3073,#3074,#3075)) ;
#1215 = EDGE_LOOP('',(#3076,#3077,#3078,#3079,#3080)) ;
#1216 = EDGE_LOOP('',(#3081,#3082,#3083,#3084)) ;
#1217 = EDGE_LOOP('',(#3085,#3086,#3087,#3088,#3089,#3090)) ;
#1218 = EDGE_LOOP('',(#3091,#3092,#3093,#3094,#3095,#3096)) ;
#1219 = EDGE_LOOP('',(#3097,#3098,#3099,#3100)) ;
#1220 = EDGE_LOOP('',(#3101,#3102,#3103,#3104,#3105)) ;
#1221 = EDGE_LOOP('',(#3106,#3107,#3108,#3109,#3110,#3111)) ;
#1222 = EDGE_LOOP('',(#3112,#3113,#3114,#3115,#3116,#3117)) ;
#1223 = EDGE_LOOP('',(#3118,#3119,#3120,#3121)) ;
#1224 = EDGE_LOOP('',(#3122,#3123,#3124,#3125,#3126)) ;
#1225 = EDGE_LOOP('',(#3127,#3128,#3129,#3130,#3131,#3132)) ;
#1226 = EDGE_LOOP('',(#3133,#3134,#3135,#3136,#3137)) ;
#1227 = EDGE_LOOP('',(#3138,#3139,#3140,#3141)) ;
#1228 = EDGE_LOOP('',(#3142,#3143,#3144,#3145,#3146,#3147)) ;
#1229 = EDGE_LOOP('',(#3148,#3149,#3150,#3151,#3152,#3153)) ;
#1230 = EDGE_LOOP('',(#3154,#3155,#3156,#3157,#3158,#3159)) ;
#1231 = EDGE_LOOP('',(#3160,#3161,#3162,#3163,#3164)) ;
#1232 = EDGE_LOOP('',(#3165,#3166,#3167,#3168)) ;
#1233 = EDGE_LOOP('',(#3169,#3170,#3171,#3172,#3173,#3174)) ;
#1234 = EDGE_LOOP('',(#3175,#3176,#3177,#3178,#3179,#3180)) ;
#1235 = EDGE_LOOP('',(#3181,#3182,#3183,#3184)) ;
#1236 = EDGE_LOOP('',(#3185,#3186,#3187,#3188,#3189)) ;
#1237 = EDGE_LOOP('',(#3190,#3191,#3192,#3193,#3194,#3195)) ;
#1238 = EDGE_LOOP('',(#3196,#3197,#3198,#3199,#3200,#3201)) ;
#1239 = EDGE_LOOP('',(#3202,#3203,#3204,#3205)) ;
#1240 = EDGE_LOOP('',(#3206,#3207,#3208,#3209,#3210)) ;
#1241 = EDGE_LOOP('',(#3211,#3212,#3213,#3214,#3215,#3216)) ;
#1242 = EDGE_LOOP('',(#3217,#3218,#3219,#3220,#3221)) ;
#1243 = EDGE_LOOP('',(#3222,#3223,#3224,#3225)) ;
#1244 = EDGE_LOOP('',(#3226,#3227,#3228,#3229,#3230,#3231)) ;
#1245 = EDGE_LOOP('',(#3232,#3233,#3234,#3235,#3236,#3237)) ;
#1246 = EDGE_LOOP('',(#3238,#3239,#3240,#3241,#3242,#3243)) ;
#1247 = EDGE_LOOP('',(#3244,#3245,#3246,#3247,#3248)) ;
#1248 = EDGE_LOOP('',(#3249,#3250,#3251,#3252)) ;
#1249 = EDGE_LOOP('',(#3253,#3254,#3255,#3256,#3257,#3258)) ;
#1250 = EDGE_LOOP('',(#3259,#3260,#3261,#3262,#3263,#3264)) ;
#1251 = EDGE_LOOP('',(#3265,#3266,#3267,#3268)) ;
#1252 = EDGE_LOOP('',(#3269,#3270,#3271,#3272,#3273)) ;
#1253 = EDGE_LOOP('',(#3274,#3275,#3276,#3277,#3278,#3279)) ;
#1254 = EDGE_LOOP('',(#3280,#3281,#3282,#3283,#3284,#3285)) ;
#1255 = EDGE_LOOP('',(#3286,#3287,#3288,#3289)) ;
#1256 = EDGE_LOOP('',(#3290,#3291,#3292,#3293,#3294)) ;
#1257 = EDGE_LOOP('',(#3295,#3296,#3297,#3298,#3299,#3300)) ;
#1258 = CIRCLE('',#3947,36.9499999999999) ;
#1259 = CIRCLE('',#3948,36.9499999999999) ;
#1260 = CIRCLE('',#3949,7.1235909466484) ;
#1261 = CIRCLE('',#3950,35.) ;
#1262 = CIRCLE('',#3952,34.8499999999999) ;
#1263 = CIRCLE('',#3953,7.27359094664848) ;
#1264 = CIRCLE('',#3954,36.8410607518303) ;
#1265 = CIRCLE('',#3955,36.8410607518303) ;
#1266 = CIRCLE('',#3960,41.0104872556708) ;
#1267 = CIRCLE('',#3961,41.0104872556708) ;
#1268 = CIRCLE('',#3962,12.6169576826623) ;
#1269 = CIRCLE('',#3963,36.984442871488) ;
#1270 = CIRCLE('',#3964,36.984442871488) ;
#1271 = CIRCLE('',#3966,40.9498221718178) ;
#1272 = CIRCLE('',#3967,40.9498221718178) ;
#1273 = CIRCLE('',#3969,36.8755027779276) ;
#1274 = CIRCLE('',#3970,36.8755027779276) ;
#1275 = CIRCLE('',#3971,12.7669576826623) ;
#1276 = CIRCLE('',#3975,0.349999999999999) ;
#1277 = CIRCLE('',#3976,35.4) ;
#1278 = CIRCLE('',#3979,0.349999999999999) ;
#1279 = CIRCLE('',#3980,35.4) ;
#1280 = CIRCLE('',#3983,0.349999999999999) ;
#1281 = CIRCLE('',#3984,35.4) ;
#1282 = CIRCLE('',#3987,0.349999999999999) ;
#1283 = CIRCLE('',#3988,35.4) ;
#1284 = CIRCLE('',#3991,0.349999999999999) ;
#1285 = CIRCLE('',#3992,35.4) ;
#1286 = CIRCLE('',#3995,0.349999999999999) ;
#1287 = CIRCLE('',#3996,35.0768144613668) ;
#1288 = CIRCLE('',#3999,0.349999999999999) ;
#1289 = CIRCLE('',#4000,33.0768144613668) ;
#1290 = CIRCLE('',#4003,0.349999999999999) ;
#1291 = CIRCLE('',#4004,31.0768144613668) ;
#1292 = CIRCLE('',#4007,0.349999999999999) ;
#1293 = CIRCLE('',#4008,29.0768144613668) ;
#1294 = CIRCLE('',#4011,0.349999999999999) ;
#1295 = CIRCLE('',#4012,27.0768144613668) ;
#1296 = CIRCLE('',#4015,0.349999999999999) ;
#1297 = CIRCLE('',#4016,25.0768144613668) ;
#1298 = CIRCLE('',#4019,0.349999999999999) ;
#1299 = CIRCLE('',#4020,23.0768144613668) ;
#1300 = CIRCLE('',#4023,0.349999999999999) ;
#1301 = CIRCLE('',#4024,21.0768144613668) ;
#1302 = CIRCLE('',#4027,0.349999999999999) ;
#1303 = CIRCLE('',#4028,19.0768144613668) ;
#1304 = CIRCLE('',#4031,0.349999999999999) ;
#1305 = CIRCLE('',#4032,17.0768144613668) ;
#1306 = CIRCLE('',#4035,0.349999999999999) ;
#1307 = CIRCLE('',#4036,15.0768144613668) ;
#1308 = CIRCLE('',#4039,0.349999999999999) ;
#1309 = CIRCLE('',#4040,13.0768144613668) ;
#1310 = CIRCLE('',#4043,0.349999999999999) ;
#1311 = CIRCLE('',#4044,11.0768144613668) ;
#1312 = CIRCLE('',#4047,0.349999999999999) ;
#1313 = CIRCLE('',#4048,9.07681446136679) ;
#1314 = CIRCLE('',#4051,0.349999999999999) ;
#1315 = CIRCLE('',#4052,7.07681446136678) ;
#1316 = CIRCLE('',#4055,0.349999999999999) ;
#1317 = CIRCLE('',#4056,5.07681446136678) ;
#1318 = CIRCLE('',#4059,0.349999999999999) ;
#1319 = CIRCLE('',#4060,3.07681446136678) ;
#1320 = CIRCLE('',#4088,7.6) ;
#1321 = CIRCLE('',#4089,7.6) ;
#1322 = CIRCLE('',#4090,7.6) ;
#1323 = CIRCLE('',#4091,7.6) ;
#1324 = CIRCLE('',#4092,7.6) ;
#1325 = CIRCLE('',#4093,7.6) ;
#1326 = CIRCLE('',#4094,7.60000000000001) ;
#1327 = CIRCLE('',#4095,7.6) ;
#1328 = CIRCLE('',#4097,7.) ;
#1329 = CIRCLE('',#4106,7.00000000000001) ;
#1330 = CIRCLE('',#4115,7.) ;
#1331 = CIRCLE('',#4123,7.) ;
#1332 = CIRCLE('',#4131,7.) ;
#1333 = CIRCLE('',#4140,35.75) ;
#1334 = CIRCLE('',#4141,35.75) ;
#1335 = CIRCLE('',#4143,35.9) ;
#1336 = CIRCLE('',#4144,35.9) ;
#1337 = CIRCLE('',#4153,2.) ;
#1338 = CIRCLE('',#4154,2.) ;
#1339 = CIRCLE('',#4155,2.) ;
#1340 = CIRCLE('',#4156,2.) ;
#1341 = CIRCLE('',#4158,2.) ;
#1342 = CIRCLE('',#4159,2.) ;
#1343 = CIRCLE('',#4160,2.) ;
#1344 = CIRCLE('',#4161,2.) ;
#1345 = CIRCLE('',#4172,41.0104872556708) ;
#1346 = CIRCLE('',#4173,41.0104872556708) ;
#1347 = CIRCLE('',#4181,0.399999999999995) ;
#1348 = CIRCLE('',#4182,0.549999999999995) ;
#1349 = CIRCLE('',#4184,0.399999999999995) ;
#1350 = CIRCLE('',#4185,0.549999999999995) ;
#1351 = CIRCLE('',#4194,0.4) ;
#1352 = CIRCLE('',#4195,0.550000000000001) ;
#1353 = CIRCLE('',#4197,0.4) ;
#1354 = CIRCLE('',#4198,0.550000000000001) ;
#1355 = CIRCLE('',#4207,0.399999999999995) ;
#1356 = CIRCLE('',#4208,0.549999999999995) ;
#1357 = CIRCLE('',#4210,0.399999999999995) ;
#1358 = CIRCLE('',#4211,0.549999999999995) ;
#1359 = CIRCLE('',#4220,0.4) ;
#1360 = CIRCLE('',#4221,0.550000000000001) ;
#1361 = CIRCLE('',#4223,0.4) ;
#1362 = CIRCLE('',#4224,0.550000000000001) ;
#1363 = CIRCLE('',#4234,0.600000000000001) ;
#1364 = CIRCLE('',#4235,0.899999999999999) ;
#1365 = CIRCLE('',#4236,0.600000000000001) ;
#1366 = CIRCLE('',#4237,0.600000000000001) ;
#1367 = CIRCLE('',#4239,0.600000000000001) ;
#1368 = CIRCLE('',#4240,1.4) ;
#1369 = CIRCLE('',#4241,0.600000000000001) ;
#1370 = CIRCLE('',#4243,0.600000000000001) ;
#1371 = CIRCLE('',#4244,0.600000000000001) ;
#1372 = CIRCLE('',#4245,1.4) ;
#1373 = CIRCLE('',#4246,0.600000000000001) ;
#1374 = CIRCLE('',#4247,0.600000000000001) ;
#1375 = CIRCLE('',#4249,0.600000000000001) ;
#1376 = CIRCLE('',#4250,0.400000000000006) ;
#1377 = CIRCLE('',#4251,0.600000000000001) ;
#1378 = CIRCLE('',#4252,0.600000000000001) ;
#1379 = CIRCLE('',#4253,0.600000000000001) ;
#1380 = CIRCLE('',#4255,0.600000000000001) ;
#1381 = CIRCLE('',#4256,0.600000000000001) ;
#1382 = CIRCLE('',#4257,0.400000000000006) ;
#1383 = CIRCLE('',#4258,0.600000000000001) ;
#1384 = CIRCLE('',#4259,0.600000000000001) ;
#1385 = CIRCLE('',#4261,0.600000000000001) ;
#1386 = CIRCLE('',#4262,0.600000000000001) ;
#1387 = CIRCLE('',#4263,0.899999999999999) ;
#1388 = CIRCLE('',#4264,0.600000000000001) ;
#1389 = CIRCLE('',#4266,0.600000000000001) ;
#1390 = CIRCLE('',#4267,1.4) ;
#1391 = CIRCLE('',#4268,0.600000000000001) ;
#1392 = CIRCLE('',#4270,0.600000000000001) ;
#1393 = CIRCLE('',#4271,0.600000000000001) ;
#1394 = CIRCLE('',#4272,1.4) ;
#1395 = CIRCLE('',#4273,0.600000000000001) ;
#1396 = CIRCLE('',#4274,0.600000000000001) ;
#1397 = CIRCLE('',#4285,0.600000000000001) ;
#1398 = CIRCLE('',#4286,0.900000000000006) ;
#1399 = CIRCLE('',#4287,0.600000000000001) ;
#1400 = CIRCLE('',#4288,0.600000000000001) ;
#1401 = CIRCLE('',#4290,0.600000000000001) ;
#1402 = CIRCLE('',#4291,1.40000000000001) ;
#1403 = CIRCLE('',#4292,0.600000000000001) ;
#1404 = CIRCLE('',#4294,0.600000000000001) ;
#1405 = CIRCLE('',#4295,0.600000000000001) ;
#1406 = CIRCLE('',#4296,1.40000000000001) ;
#1407 = CIRCLE('',#4297,0.600000000000001) ;
#1408 = CIRCLE('',#4298,0.600000000000001) ;
#1409 = CIRCLE('',#4300,0.600000000000001) ;
#1410 = CIRCLE('',#4301,0.399999999999999) ;
#1411 = CIRCLE('',#4302,0.600000000000001) ;
#1412 = CIRCLE('',#4303,0.600000000000001) ;
#1413 = CIRCLE('',#4304,0.600000000000001) ;
#1414 = CIRCLE('',#4306,0.600000000000001) ;
#1415 = CIRCLE('',#4307,0.600000000000001) ;
#1416 = CIRCLE('',#4308,0.400000000000002) ;
#1417 = CIRCLE('',#4309,0.600000000000001) ;
#1418 = CIRCLE('',#4310,0.600000000000001) ;
#1419 = CIRCLE('',#4312,0.600000000000001) ;
#1420 = CIRCLE('',#4313,0.600000000000001) ;
#1421 = CIRCLE('',#4314,0.900000000000006) ;
#1422 = CIRCLE('',#4315,0.600000000000001) ;
#1423 = CIRCLE('',#4317,0.600000000000001) ;
#1424 = CIRCLE('',#4318,1.40000000000001) ;
#1425 = CIRCLE('',#4319,0.600000000000001) ;
#1426 = CIRCLE('',#4321,0.600000000000001) ;
#1427 = CIRCLE('',#4322,0.600000000000001) ;
#1428 = CIRCLE('',#4323,1.40000000000001) ;
#1429 = CIRCLE('',#4324,0.600000000000001) ;
#1430 = CIRCLE('',#4325,0.600000000000001) ;
#1431 = CIRCLE('',#4336,0.600000000000001) ;
#1432 = CIRCLE('',#4337,0.9) ;
#1433 = CIRCLE('',#4338,0.600000000000001) ;
#1434 = CIRCLE('',#4339,0.600000000000001) ;
#1435 = CIRCLE('',#4341,0.600000000000001) ;
#1436 = CIRCLE('',#4342,1.4) ;
#1437 = CIRCLE('',#4343,0.600000000000001) ;
#1438 = CIRCLE('',#4345,0.600000000000001) ;
#1439 = CIRCLE('',#4346,0.600000000000001) ;
#1440 = CIRCLE('',#4347,1.4) ;
#1441 = CIRCLE('',#4348,0.600000000000001) ;
#1442 = CIRCLE('',#4349,0.600000000000001) ;
#1443 = CIRCLE('',#4351,0.600000000000001) ;
#1444 = CIRCLE('',#4352,0.400000000000006) ;
#1445 = CIRCLE('',#4353,0.600000000000001) ;
#1446 = CIRCLE('',#4354,0.600000000000001) ;
#1447 = CIRCLE('',#4355,0.600000000000001) ;
#1448 = CIRCLE('',#4357,0.600000000000001) ;
#1449 = CIRCLE('',#4358,0.600000000000001) ;
#1450 = CIRCLE('',#4359,0.400000000000006) ;
#1451 = CIRCLE('',#4360,0.600000000000001) ;
#1452 = CIRCLE('',#4361,0.600000000000001) ;
#1453 = CIRCLE('',#4363,0.600000000000001) ;
#1454 = CIRCLE('',#4364,0.600000000000001) ;
#1455 = CIRCLE('',#4365,0.9) ;
#1456 = CIRCLE('',#4366,0.600000000000001) ;
#1457 = CIRCLE('',#4368,0.600000000000001) ;
#1458 = CIRCLE('',#4369,1.4) ;
#1459 = CIRCLE('',#4370,0.600000000000001) ;
#1460 = CIRCLE('',#4372,0.600000000000001) ;
#1461 = CIRCLE('',#4373,0.600000000000001) ;
#1462 = CIRCLE('',#4374,1.4) ;
#1463 = CIRCLE('',#4375,0.600000000000001) ;
#1464 = CIRCLE('',#4376,0.600000000000001) ;
#1465 = CIRCLE('',#4387,0.600000000000001) ;
#1466 = CIRCLE('',#4388,0.899999999999999) ;
#1467 = CIRCLE('',#4389,0.600000000000001) ;
#1468 = CIRCLE('',#4390,0.600000000000001) ;
#1469 = CIRCLE('',#4392,0.600000000000001) ;
#1470 = CIRCLE('',#4393,1.4) ;
#1471 = CIRCLE('',#4394,0.600000000000001) ;
#1472 = CIRCLE('',#4396,0.600000000000001) ;
#1473 = CIRCLE('',#4397,0.600000000000001) ;
#1474 = CIRCLE('',#4398,1.4) ;
#1475 = CIRCLE('',#4399,0.600000000000001) ;
#1476 = CIRCLE('',#4400,0.600000000000001) ;
#1477 = CIRCLE('',#4402,0.600000000000001) ;
#1478 = CIRCLE('',#4403,0.399999999999999) ;
#1479 = CIRCLE('',#4404,0.600000000000001) ;
#1480 = CIRCLE('',#4405,0.600000000000001) ;
#1481 = CIRCLE('',#4406,0.600000000000001) ;
#1482 = CIRCLE('',#4408,0.600000000000001) ;
#1483 = CIRCLE('',#4409,0.600000000000001) ;
#1484 = CIRCLE('',#4410,0.400000000000002) ;
#1485 = CIRCLE('',#4411,0.600000000000001) ;
#1486 = CIRCLE('',#4412,0.600000000000001) ;
#1487 = CIRCLE('',#4414,0.600000000000001) ;
#1488 = CIRCLE('',#4415,0.600000000000001) ;
#1489 = CIRCLE('',#4416,0.899999999999999) ;
#1490 = CIRCLE('',#4417,0.600000000000001) ;
#1491 = CIRCLE('',#4419,0.600000000000001) ;
#1492 = CIRCLE('',#4420,1.4) ;
#1493 = CIRCLE('',#4421,0.600000000000001) ;
#1494 = CIRCLE('',#4423,0.600000000000001) ;
#1495 = CIRCLE('',#4424,0.600000000000001) ;
#1496 = CIRCLE('',#4425,1.4) ;
#1497 = CIRCLE('',#4426,0.600000000000001) ;
#1498 = CIRCLE('',#4427,0.600000000000001) ;
#1499 = VERTEX_POINT('',#5608) ;
#1500 = VERTEX_POINT('',#5609) ;
#1501 = VERTEX_POINT('',#5612) ;
#1502 = VERTEX_POINT('',#5616) ;
#1503 = VERTEX_POINT('',#5618) ;
#1504 = VERTEX_POINT('',#5620) ;
#1505 = VERTEX_POINT('',#5628) ;
#1506 = VERTEX_POINT('',#5629) ;
#1507 = VERTEX_POINT('',#5632) ;
#1508 = VERTEX_POINT('',#5634) ;
#1509 = VERTEX_POINT('',#5638) ;
#1510 = VERTEX_POINT('',#5640) ;
#1511 = VERTEX_POINT('',#5644) ;
#1512 = VERTEX_POINT('',#5645) ;
#1513 = VERTEX_POINT('',#5653) ;
#1514 = VERTEX_POINT('',#5658) ;
#1515 = VERTEX_POINT('',#5663) ;
#1516 = VERTEX_POINT('',#5668) ;
#1517 = VERTEX_POINT('',#5673) ;
#1518 = VERTEX_POINT('',#5678) ;
#1519 = VERTEX_POINT('',#5683) ;
#1520 = VERTEX_POINT('',#5688) ;
#1521 = VERTEX_POINT('',#5693) ;
#1522 = VERTEX_POINT('',#5698) ;
#1523 = VERTEX_POINT('',#5703) ;
#1524 = VERTEX_POINT('',#5708) ;
#1525 = VERTEX_POINT('',#5713) ;
#1526 = VERTEX_POINT('',#5718) ;
#1527 = VERTEX_POINT('',#5723) ;
#1528 = VERTEX_POINT('',#5728) ;
#1529 = VERTEX_POINT('',#5733) ;
#1530 = VERTEX_POINT('',#5738) ;
#1531 = VERTEX_POINT('',#5743) ;
#1532 = VERTEX_POINT('',#5748) ;
#1533 = VERTEX_POINT('',#5753) ;
#1534 = VERTEX_POINT('',#5758) ;
#1535 = VERTEX_POINT('',#5788) ;
#1536 = VERTEX_POINT('',#5790) ;
#1537 = VERTEX_POINT('',#5792) ;
#1538 = VERTEX_POINT('',#5797) ;
#1539 = VERTEX_POINT('',#5799) ;
#1540 = VERTEX_POINT('',#5802) ;
#1541 = VERTEX_POINT('',#5804) ;
#1542 = VERTEX_POINT('',#5861) ;
#1543 = VERTEX_POINT('',#5866) ;
#1544 = VERTEX_POINT('',#5930) ;
#1545 = VERTEX_POINT('',#5931) ;
#1546 = VERTEX_POINT('',#5952) ;
#1547 = VERTEX_POINT('',#5957) ;
#1548 = VERTEX_POINT('',#5959) ;
#1549 = VERTEX_POINT('',#5978) ;
#1550 = VERTEX_POINT('',#6040) ;
#1551 = VERTEX_POINT('',#6079) ;
#1552 = VERTEX_POINT('',#6080) ;
#1553 = VERTEX_POINT('',#6137) ;
#1554 = VERTEX_POINT('',#6142) ;
#1555 = VERTEX_POINT('',#6144) ;
#1556 = VERTEX_POINT('',#6210) ;
#1557 = VERTEX_POINT('',#6211) ;
#1558 = VERTEX_POINT('',#6269) ;
#1559 = VERTEX_POINT('',#6274) ;
#1560 = VERTEX_POINT('',#6276) ;
#1561 = VERTEX_POINT('',#6341) ;
#1562 = VERTEX_POINT('',#6342) ;
#1563 = VERTEX_POINT('',#6399) ;
#1564 = VERTEX_POINT('',#6404) ;
#1565 = VERTEX_POINT('',#6406) ;
#1566 = VERTEX_POINT('',#6472) ;
#1567 = VERTEX_POINT('',#6473) ;
#1568 = VERTEX_POINT('',#6487) ;
#1569 = VERTEX_POINT('',#6500) ;
#1570 = VERTEX_POINT('',#6549) ;
#1571 = VERTEX_POINT('',#6550) ;
#1572 = VERTEX_POINT('',#6645) ;
#1573 = VERTEX_POINT('',#6658) ;
#1574 = VERTEX_POINT('',#6660) ;
#1575 = VERTEX_POINT('',#6676) ;
#1576 = VERTEX_POINT('',#6738) ;
#1577 = VERTEX_POINT('',#6819) ;
#1578 = VERTEX_POINT('',#6826) ;
#1579 = VERTEX_POINT('',#6841) ;
#1580 = VERTEX_POINT('',#7110) ;
#1581 = VERTEX_POINT('',#7111) ;
#1582 = VERTEX_POINT('',#7125) ;
#1583 = VERTEX_POINT('',#7138) ;
#1584 = VERTEX_POINT('',#7187) ;
#1585 = VERTEX_POINT('',#7188) ;
#1586 = VERTEX_POINT('',#7283) ;
#1587 = VERTEX_POINT('',#7296) ;
#1588 = VERTEX_POINT('',#7298) ;
#1589 = VERTEX_POINT('',#7314) ;
#1590 = VERTEX_POINT('',#7376) ;
#1591 = VERTEX_POINT('',#7457) ;
#1592 = VERTEX_POINT('',#7464) ;
#1593 = VERTEX_POINT('',#7479) ;
#1594 = VERTEX_POINT('',#7748) ;
#1595 = VERTEX_POINT('',#7749) ;
#1596 = VERTEX_POINT('',#7763) ;
#1597 = VERTEX_POINT('',#7776) ;
#1598 = VERTEX_POINT('',#7825) ;
#1599 = VERTEX_POINT('',#7826) ;
#1600 = VERTEX_POINT('',#7921) ;
#1601 = VERTEX_POINT('',#7934) ;
#1602 = VERTEX_POINT('',#7936) ;
#1603 = VERTEX_POINT('',#7952) ;
#1604 = VERTEX_POINT('',#8014) ;
#1605 = VERTEX_POINT('',#8095) ;
#1606 = VERTEX_POINT('',#8102) ;
#1607 = VERTEX_POINT('',#8117) ;
#1608 = VERTEX_POINT('',#8385) ;
#1609 = VERTEX_POINT('',#8386) ;
#1610 = VERTEX_POINT('',#8400) ;
#1611 = VERTEX_POINT('',#8413) ;
#1612 = VERTEX_POINT('',#8462) ;
#1613 = VERTEX_POINT('',#8463) ;
#1614 = VERTEX_POINT('',#8558) ;
#1615 = VERTEX_POINT('',#8571) ;
#1616 = VERTEX_POINT('',#8573) ;
#1617 = VERTEX_POINT('',#8589) ;
#1618 = VERTEX_POINT('',#8651) ;
#1619 = VERTEX_POINT('',#8732) ;
#1620 = VERTEX_POINT('',#8739) ;
#1621 = VERTEX_POINT('',#8754) ;
#1622 = VERTEX_POINT('',#9022) ;
#1623 = VERTEX_POINT('',#9023) ;
#1624 = VERTEX_POINT('',#9037) ;
#1625 = VERTEX_POINT('',#9050) ;
#1626 = VERTEX_POINT('',#9099) ;
#1627 = VERTEX_POINT('',#9100) ;
#1628 = VERTEX_POINT('',#9195) ;
#1629 = VERTEX_POINT('',#9208) ;
#1630 = VERTEX_POINT('',#9210) ;
#1631 = VERTEX_POINT('',#9226) ;
#1632 = VERTEX_POINT('',#9288) ;
#1633 = VERTEX_POINT('',#9369) ;
#1634 = VERTEX_POINT('',#9376) ;
#1635 = VERTEX_POINT('',#9391) ;
#1636 = VERTEX_POINT('',#9660) ;
#1637 = VERTEX_POINT('',#9662) ;
#1638 = VERTEX_POINT('',#9666) ;
#1639 = VERTEX_POINT('',#9668) ;
#1640 = VERTEX_POINT('',#9675) ;
#1641 = VERTEX_POINT('',#9676) ;
#1642 = VERTEX_POINT('',#9678) ;
#1643 = VERTEX_POINT('',#9680) ;
#1644 = VERTEX_POINT('',#9684) ;
#1645 = VERTEX_POINT('',#9685) ;
#1646 = VERTEX_POINT('',#9687) ;
#1647 = VERTEX_POINT('',#9689) ;
#1648 = VERTEX_POINT('',#9693) ;
#1649 = VERTEX_POINT('',#9694) ;
#1650 = VERTEX_POINT('',#9696) ;
#1651 = VERTEX_POINT('',#9698) ;
#1652 = VERTEX_POINT('',#9702) ;
#1653 = VERTEX_POINT('',#9703) ;
#1654 = VERTEX_POINT('',#9705) ;
#1655 = VERTEX_POINT('',#9707) ;
#1656 = VERTEX_POINT('',#9730) ;
#1657 = VERTEX_POINT('',#9732) ;
#1658 = VERTEX_POINT('',#9736) ;
#1659 = VERTEX_POINT('',#9737) ;
#1660 = VERTEX_POINT('',#9739) ;
#1661 = VERTEX_POINT('',#9741) ;
#1662 = VERTEX_POINT('',#9743) ;
#1663 = VERTEX_POINT('',#9745) ;
#1664 = VERTEX_POINT('',#9747) ;
#1665 = VERTEX_POINT('',#9749) ;
#1666 = VERTEX_POINT('',#9753) ;
#1667 = VERTEX_POINT('',#9754) ;
#1668 = VERTEX_POINT('',#9756) ;
#1669 = VERTEX_POINT('',#9758) ;
#1670 = VERTEX_POINT('',#9760) ;
#1671 = VERTEX_POINT('',#9762) ;
#1672 = VERTEX_POINT('',#9764) ;
#1673 = VERTEX_POINT('',#9766) ;
#1674 = VERTEX_POINT('',#9782) ;
#1675 = VERTEX_POINT('',#9783) ;
#1676 = VERTEX_POINT('',#9788) ;
#1677 = VERTEX_POINT('',#9790) ;
#1678 = VERTEX_POINT('',#9798) ;
#1679 = VERTEX_POINT('',#9800) ;
#1680 = VERTEX_POINT('',#9804) ;
#1681 = VERTEX_POINT('',#9806) ;
#1682 = VERTEX_POINT('',#9815) ;
#1683 = VERTEX_POINT('',#9816) ;
#1684 = VERTEX_POINT('',#9821) ;
#1685 = VERTEX_POINT('',#9823) ;
#1686 = VERTEX_POINT('',#9831) ;
#1687 = VERTEX_POINT('',#9833) ;
#1688 = VERTEX_POINT('',#9837) ;
#1689 = VERTEX_POINT('',#9839) ;
#1690 = VERTEX_POINT('',#9848) ;
#1691 = VERTEX_POINT('',#9849) ;
#1692 = VERTEX_POINT('',#9854) ;
#1693 = VERTEX_POINT('',#9856) ;
#1694 = VERTEX_POINT('',#9864) ;
#1695 = VERTEX_POINT('',#9866) ;
#1696 = VERTEX_POINT('',#9870) ;
#1697 = VERTEX_POINT('',#9872) ;
#1698 = VERTEX_POINT('',#9881) ;
#1699 = VERTEX_POINT('',#9882) ;
#1700 = VERTEX_POINT('',#9887) ;
#1701 = VERTEX_POINT('',#9889) ;
#1702 = VERTEX_POINT('',#9897) ;
#1703 = VERTEX_POINT('',#9899) ;
#1704 = VERTEX_POINT('',#9903) ;
#1705 = VERTEX_POINT('',#9905) ;
#1706 = VERTEX_POINT('',#9915) ;
#1707 = VERTEX_POINT('',#9917) ;
#1708 = VERTEX_POINT('',#9919) ;
#1709 = VERTEX_POINT('',#9923) ;
#1710 = VERTEX_POINT('',#9925) ;
#1711 = VERTEX_POINT('',#9929) ;
#1712 = VERTEX_POINT('',#9930) ;
#1713 = VERTEX_POINT('',#9933) ;
#1714 = VERTEX_POINT('',#9935) ;
#1715 = VERTEX_POINT('',#9939) ;
#1716 = VERTEX_POINT('',#9940) ;
#1717 = VERTEX_POINT('',#9942) ;
#1718 = VERTEX_POINT('',#9944) ;
#1719 = VERTEX_POINT('',#9949) ;
#1720 = VERTEX_POINT('',#9950) ;
#1721 = VERTEX_POINT('',#9953) ;
#1722 = VERTEX_POINT('',#9955) ;
#1723 = VERTEX_POINT('',#9959) ;
#1724 = VERTEX_POINT('',#9960) ;
#1725 = VERTEX_POINT('',#9963) ;
#1726 = VERTEX_POINT('',#9967) ;
#1727 = VERTEX_POINT('',#9969) ;
#1728 = VERTEX_POINT('',#9973) ;
#1729 = VERTEX_POINT('',#9974) ;
#1730 = VERTEX_POINT('',#9977) ;
#1731 = VERTEX_POINT('',#9979) ;
#1732 = VERTEX_POINT('',#10000) ;
#1733 = VERTEX_POINT('',#10002) ;
#1734 = VERTEX_POINT('',#10004) ;
#1735 = VERTEX_POINT('',#10008) ;
#1736 = VERTEX_POINT('',#10010) ;
#1737 = VERTEX_POINT('',#10014) ;
#1738 = VERTEX_POINT('',#10015) ;
#1739 = VERTEX_POINT('',#10018) ;
#1740 = VERTEX_POINT('',#10020) ;
#1741 = VERTEX_POINT('',#10024) ;
#1742 = VERTEX_POINT('',#10025) ;
#1743 = VERTEX_POINT('',#10027) ;
#1744 = VERTEX_POINT('',#10029) ;
#1745 = VERTEX_POINT('',#10034) ;
#1746 = VERTEX_POINT('',#10035) ;
#1747 = VERTEX_POINT('',#10038) ;
#1748 = VERTEX_POINT('',#10040) ;
#1749 = VERTEX_POINT('',#10044) ;
#1750 = VERTEX_POINT('',#10045) ;
#1751 = VERTEX_POINT('',#10048) ;
#1752 = VERTEX_POINT('',#10052) ;
#1753 = VERTEX_POINT('',#10054) ;
#1754 = VERTEX_POINT('',#10058) ;
#1755 = VERTEX_POINT('',#10059) ;
#1756 = VERTEX_POINT('',#10062) ;
#1757 = VERTEX_POINT('',#10064) ;
#1758 = VERTEX_POINT('',#10085) ;
#1759 = VERTEX_POINT('',#10087) ;
#1760 = VERTEX_POINT('',#10089) ;
#1761 = VERTEX_POINT('',#10093) ;
#1762 = VERTEX_POINT('',#10095) ;
#1763 = VERTEX_POINT('',#10099) ;
#1764 = VERTEX_POINT('',#10100) ;
#1765 = VERTEX_POINT('',#10103) ;
#1766 = VERTEX_POINT('',#10105) ;
#1767 = VERTEX_POINT('',#10109) ;
#1768 = VERTEX_POINT('',#10110) ;
#1769 = VERTEX_POINT('',#10112) ;
#1770 = VERTEX_POINT('',#10114) ;
#1771 = VERTEX_POINT('',#10119) ;
#1772 = VERTEX_POINT('',#10120) ;
#1773 = VERTEX_POINT('',#10123) ;
#1774 = VERTEX_POINT('',#10125) ;
#1775 = VERTEX_POINT('',#10129) ;
#1776 = VERTEX_POINT('',#10130) ;
#1777 = VERTEX_POINT('',#10133) ;
#1778 = VERTEX_POINT('',#10137) ;
#1779 = VERTEX_POINT('',#10139) ;
#1780 = VERTEX_POINT('',#10143) ;
#1781 = VERTEX_POINT('',#10144) ;
#1782 = VERTEX_POINT('',#10147) ;
#1783 = VERTEX_POINT('',#10149) ;
#1784 = VERTEX_POINT('',#10170) ;
#1785 = VERTEX_POINT('',#10172) ;
#1786 = VERTEX_POINT('',#10174) ;
#1787 = VERTEX_POINT('',#10178) ;
#1788 = VERTEX_POINT('',#10180) ;
#1789 = VERTEX_POINT('',#10184) ;
#1790 = VERTEX_POINT('',#10185) ;
#1791 = VERTEX_POINT('',#10188) ;
#1792 = VERTEX_POINT('',#10190) ;
#1793 = VERTEX_POINT('',#10194) ;
#1794 = VERTEX_POINT('',#10195) ;
#1795 = VERTEX_POINT('',#10197) ;
#1796 = VERTEX_POINT('',#10199) ;
#1797 = VERTEX_POINT('',#10204) ;
#1798 = VERTEX_POINT('',#10205) ;
#1799 = VERTEX_POINT('',#10208) ;
#1800 = VERTEX_POINT('',#10210) ;
#1801 = VERTEX_POINT('',#10214) ;
#1802 = VERTEX_POINT('',#10215) ;
#1803 = VERTEX_POINT('',#10218) ;
#1804 = VERTEX_POINT('',#10222) ;
#1805 = VERTEX_POINT('',#10224) ;
#1806 = VERTEX_POINT('',#10228) ;
#1807 = VERTEX_POINT('',#10229) ;
#1808 = VERTEX_POINT('',#10232) ;
#1809 = VERTEX_POINT('',#10234) ;
#1810 = EDGE_CURVE('',#1499,#1500,#1258,.T.) ;
#1811 = EDGE_CURVE('',#1500,#1499,#1259,.T.) ;
#1812 = EDGE_CURVE('',#1500,#1501,#1260,.T.) ;
#1813 = EDGE_CURVE('',#1501,#1501,#1261,.T.) ;
#1814 = EDGE_CURVE('',#1502,#1502,#1262,.T.) ;
#1815 = EDGE_CURVE('',#1502,#1503,#1263,.T.) ;
#1816 = EDGE_CURVE('',#1503,#1504,#1264,.T.) ;
#1817 = EDGE_CURVE('',#1504,#1503,#1265,.T.) ;
#1818 = EDGE_CURVE('',#1499,#1504,#532,.T.) ;
#1819 = EDGE_CURVE('',#1505,#1506,#1266,.T.) ;
#1820 = EDGE_CURVE('',#1506,#1505,#1267,.T.) ;
#1821 = EDGE_CURVE('',#1506,#1507,#1268,.T.) ;
#1822 = EDGE_CURVE('',#1507,#1508,#1269,.T.) ;
#1823 = EDGE_CURVE('',#1508,#1507,#1270,.T.) ;
#1824 = EDGE_CURVE('',#1505,#1509,#533,.T.) ;
#1825 = EDGE_CURVE('',#1510,#1509,#1271,.T.) ;
#1826 = EDGE_CURVE('',#1509,#1510,#1272,.T.) ;
#1827 = EDGE_CURVE('',#1511,#1512,#1273,.T.) ;
#1828 = EDGE_CURVE('',#1512,#1511,#1274,.T.) ;
#1829 = EDGE_CURVE('',#1512,#1510,#1275,.T.) ;
#1830 = EDGE_CURVE('',#1511,#1508,#534,.T.) ;
#1831 = EDGE_CURVE('',#1513,#1513,#1276,.T.) ;
#1832 = EDGE_CURVE('',#1513,#1513,#1277,.T.) ;
#1833 = EDGE_CURVE('',#1514,#1514,#1278,.T.) ;
#1834 = EDGE_CURVE('',#1514,#1514,#1279,.T.) ;
#1835 = EDGE_CURVE('',#1515,#1515,#1280,.T.) ;
#1836 = EDGE_CURVE('',#1515,#1515,#1281,.T.) ;
#1837 = EDGE_CURVE('',#1516,#1516,#1282,.T.) ;
#1838 = EDGE_CURVE('',#1516,#1516,#1283,.T.) ;
#1839 = EDGE_CURVE('',#1517,#1517,#1284,.T.) ;
#1840 = EDGE_CURVE('',#1517,#1517,#1285,.T.) ;
#1841 = EDGE_CURVE('',#1518,#1518,#1286,.T.) ;
#1842 = EDGE_CURVE('',#1518,#1518,#1287,.T.) ;
#1843 = EDGE_CURVE('',#1519,#1519,#1288,.T.) ;
#1844 = EDGE_CURVE('',#1519,#1519,#1289,.T.) ;
#1845 = EDGE_CURVE('',#1520,#1520,#1290,.T.) ;
#1846 = EDGE_CURVE('',#1520,#1520,#1291,.T.) ;
#1847 = EDGE_CURVE('',#1521,#1521,#1292,.T.) ;
#1848 = EDGE_CURVE('',#1521,#1521,#1293,.T.) ;
#1849 = EDGE_CURVE('',#1522,#1522,#1294,.T.) ;
#1850 = EDGE_CURVE('',#1522,#1522,#1295,.T.) ;
#1851 = EDGE_CURVE('',#1523,#1523,#1296,.T.) ;
#1852 = EDGE_CURVE('',#1523,#1523,#1297,.T.) ;
#1853 = EDGE_CURVE('',#1524,#1524,#1298,.T.) ;
#1854 = EDGE_CURVE('',#1524,#1524,#1299,.T.) ;
#1855 = EDGE_CURVE('',#1525,#1525,#1300,.T.) ;
#1856 = EDGE_CURVE('',#1525,#1525,#1301,.T.) ;
#1857 = EDGE_CURVE('',#1526,#1526,#1302,.T.) ;
#1858 = EDGE_CURVE('',#1526,#1526,#1303,.T.) ;
#1859 = EDGE_CURVE('',#1527,#1527,#1304,.T.) ;
#1860 = EDGE_CURVE('',#1527,#1527,#1305,.T.) ;
#1861 = EDGE_CURVE('',#1528,#1528,#1306,.T.) ;
#1862 = EDGE_CURVE('',#1528,#1528,#1307,.T.) ;
#1863 = EDGE_CURVE('',#1529,#1529,#1308,.T.) ;
#1864 = EDGE_CURVE('',#1529,#1529,#1309,.T.) ;
#1865 = EDGE_CURVE('',#1530,#1530,#1310,.T.) ;
#1866 = EDGE_CURVE('',#1530,#1530,#1311,.T.) ;
#1867 = EDGE_CURVE('',#1531,#1531,#1312,.T.) ;
#1868 = EDGE_CURVE('',#1531,#1531,#1313,.T.) ;
#1869 = EDGE_CURVE('',#1532,#1532,#1314,.T.) ;
#1870 = EDGE_CURVE('',#1532,#1532,#1315,.T.) ;
#1871 = EDGE_CURVE('',#1533,#1533,#1316,.T.) ;
#1872 = EDGE_CURVE('',#1533,#1533,#1317,.T.) ;
#1873 = EDGE_CURVE('',#1534,#1534,#1318,.T.) ;
#1874 = EDGE_CURVE('',#1534,#1534,#1319,.T.) ;
#1875 = EDGE_CURVE('',#1535,#1535,#1320,.T.) ;
#1876 = EDGE_CURVE('',#1535,#1536,#535,.T.) ;
#1877 = EDGE_CURVE('',#1536,#1537,#51,.T.) ;
#1878 = EDGE_CURVE('',#1538,#1537,#1321,.T.) ;
#1879 = EDGE_CURVE('',#1538,#1539,#536,.T.) ;
#1880 = EDGE_CURVE('',#1539,#1539,#1322,.T.) ;
#1881 = EDGE_CURVE('',#1540,#1538,#1323,.T.) ;
#1882 = EDGE_CURVE('',#1540,#1541,#52,.T.) ;
#1883 = EDGE_CURVE('',#1541,#1542,#53,.T.) ;
#1884 = EDGE_CURVE('',#1542,#1543,#537,.T.) ;
#1885 = EDGE_CURVE('',#1543,#1536,#54,.T.) ;
#1886 = EDGE_CURVE('',#1544,#1545,#55,.T.) ;
#1887 = EDGE_CURVE('',#1545,#1546,#56,.T.) ;
#1888 = EDGE_CURVE('',#1546,#1547,#538,.T.) ;
#1889 = EDGE_CURVE('',#1547,#1548,#57,.T.) ;
#1890 = EDGE_CURVE('',#1548,#1549,#58,.T.) ;
#1891 = EDGE_CURVE('',#1550,#1549,#1324,.T.) ;
#1892 = EDGE_CURVE('',#1550,#1544,#59,.T.) ;
#1893 = EDGE_CURVE('',#1551,#1552,#60,.T.) ;
#1894 = EDGE_CURVE('',#1552,#1553,#61,.T.) ;
#1895 = EDGE_CURVE('',#1553,#1554,#539,.T.) ;
#1896 = EDGE_CURVE('',#1554,#1555,#62,.T.) ;
#1897 = EDGE_CURVE('',#1551,#1555,#1325,.T.) ;
#1898 = EDGE_CURVE('',#1556,#1557,#63,.T.) ;
#1899 = EDGE_CURVE('',#1557,#1558,#64,.T.) ;
#1900 = EDGE_CURVE('',#1558,#1559,#540,.T.) ;
#1901 = EDGE_CURVE('',#1559,#1560,#65,.T.) ;
#1902 = EDGE_CURVE('',#1556,#1560,#1326,.T.) ;
#1903 = EDGE_CURVE('',#1561,#1562,#66,.T.) ;
#1904 = EDGE_CURVE('',#1562,#1563,#67,.T.) ;
#1905 = EDGE_CURVE('',#1563,#1564,#541,.T.) ;
#1906 = EDGE_CURVE('',#1564,#1565,#68,.T.) ;
#1907 = EDGE_CURVE('',#1561,#1565,#1327,.T.) ;
#1908 = EDGE_CURVE('',#1566,#1567,#542,.T.) ;
#1909 = EDGE_CURVE('',#1566,#1540,#69,.T.) ;
#1910 = EDGE_CURVE('',#1537,#1568,#70,.T.) ;
#1911 = EDGE_CURVE('',#1569,#1568,#543,.T.) ;
#1912 = EDGE_CURVE('',#1567,#1569,#1328,.T.) ;
#1913 = EDGE_CURVE('',#1570,#1571,#71,.T.) ;
#1914 = EDGE_CURVE('',#1571,#1566,#72,.T.) ;
#1915 = EDGE_CURVE('',#1567,#1572,#73,.T.) ;
#1916 = EDGE_CURVE('',#1572,#1573,#21,.T.) ;
#1917 = EDGE_CURVE('',#1573,#1574,#11,.T.) ;
#1918 = EDGE_CURVE('',#1574,#1575,#22,.T.) ;
#1919 = EDGE_CURVE('',#1575,#1570,#74,.T.) ;
#1920 = EDGE_CURVE('',#1568,#1576,#75,.T.) ;
#1921 = EDGE_CURVE('',#1576,#1577,#76,.T.) ;
#1922 = EDGE_CURVE('',#1577,#1578,#77,.T.) ;
#1923 = EDGE_CURVE('',#1579,#1578,#12,.T.) ;
#1924 = EDGE_CURVE('',#1579,#1569,#78,.T.) ;
#1925 = EDGE_CURVE('',#1573,#1579,#544,.T.) ;
#1926 = EDGE_CURVE('',#1574,#1578,#545,.T.) ;
#1927 = EDGE_CURVE('',#1570,#1577,#546,.T.) ;
#1928 = EDGE_CURVE('',#1542,#1571,#79,.T.) ;
#1929 = EDGE_CURVE('',#1576,#1543,#80,.T.) ;
#1930 = EDGE_CURVE('',#1580,#1581,#547,.T.) ;
#1931 = EDGE_CURVE('',#1580,#1551,#81,.T.) ;
#1932 = EDGE_CURVE('',#1555,#1582,#82,.T.) ;
#1933 = EDGE_CURVE('',#1583,#1582,#548,.T.) ;
#1934 = EDGE_CURVE('',#1581,#1583,#1329,.T.) ;
#1935 = EDGE_CURVE('',#1584,#1585,#83,.T.) ;
#1936 = EDGE_CURVE('',#1585,#1580,#84,.T.) ;
#1937 = EDGE_CURVE('',#1581,#1586,#85,.T.) ;
#1938 = EDGE_CURVE('',#1586,#1587,#23,.T.) ;
#1939 = EDGE_CURVE('',#1587,#1588,#13,.T.) ;
#1940 = EDGE_CURVE('',#1588,#1589,#24,.T.) ;
#1941 = EDGE_CURVE('',#1589,#1584,#86,.T.) ;
#1942 = EDGE_CURVE('',#1582,#1590,#87,.T.) ;
#1943 = EDGE_CURVE('',#1590,#1591,#88,.T.) ;
#1944 = EDGE_CURVE('',#1591,#1592,#89,.T.) ;
#1945 = EDGE_CURVE('',#1593,#1592,#14,.T.) ;
#1946 = EDGE_CURVE('',#1593,#1583,#90,.T.) ;
#1947 = EDGE_CURVE('',#1587,#1593,#549,.T.) ;
#1948 = EDGE_CURVE('',#1588,#1592,#550,.T.) ;
#1949 = EDGE_CURVE('',#1584,#1591,#551,.T.) ;
#1950 = EDGE_CURVE('',#1553,#1585,#91,.T.) ;
#1951 = EDGE_CURVE('',#1590,#1554,#92,.T.) ;
#1952 = EDGE_CURVE('',#1594,#1595,#552,.T.) ;
#1953 = EDGE_CURVE('',#1594,#1556,#93,.T.) ;
#1954 = EDGE_CURVE('',#1560,#1596,#94,.T.) ;
#1955 = EDGE_CURVE('',#1597,#1596,#553,.T.) ;
#1956 = EDGE_CURVE('',#1595,#1597,#1330,.T.) ;
#1957 = EDGE_CURVE('',#1598,#1599,#95,.T.) ;
#1958 = EDGE_CURVE('',#1599,#1594,#96,.T.) ;
#1959 = EDGE_CURVE('',#1595,#1600,#97,.T.) ;
#1960 = EDGE_CURVE('',#1600,#1601,#25,.T.) ;
#1961 = EDGE_CURVE('',#1601,#1602,#15,.T.) ;
#1962 = EDGE_CURVE('',#1602,#1603,#26,.T.) ;
#1963 = EDGE_CURVE('',#1603,#1598,#98,.T.) ;
#1964 = EDGE_CURVE('',#1596,#1604,#99,.T.) ;
#1965 = EDGE_CURVE('',#1604,#1605,#100,.T.) ;
#1966 = EDGE_CURVE('',#1605,#1606,#101,.T.) ;
#1967 = EDGE_CURVE('',#1607,#1606,#16,.T.) ;
#1968 = EDGE_CURVE('',#1607,#1597,#102,.T.) ;
#1969 = EDGE_CURVE('',#1601,#1607,#554,.T.) ;
#1970 = EDGE_CURVE('',#1602,#1606,#555,.T.) ;
#1971 = EDGE_CURVE('',#1598,#1605,#556,.T.) ;
#1972 = EDGE_CURVE('',#1558,#1599,#103,.T.) ;
#1973 = EDGE_CURVE('',#1604,#1559,#104,.T.) ;
#1974 = EDGE_CURVE('',#1608,#1609,#557,.T.) ;
#1975 = EDGE_CURVE('',#1608,#1550,#105,.T.) ;
#1976 = EDGE_CURVE('',#1549,#1610,#106,.T.) ;
#1977 = EDGE_CURVE('',#1611,#1610,#558,.T.) ;
#1978 = EDGE_CURVE('',#1609,#1611,#1331,.T.) ;
#1979 = EDGE_CURVE('',#1612,#1613,#107,.T.) ;
#1980 = EDGE_CURVE('',#1613,#1608,#108,.T.) ;
#1981 = EDGE_CURVE('',#1609,#1614,#109,.T.) ;
#1982 = EDGE_CURVE('',#1614,#1615,#27,.T.) ;
#1983 = EDGE_CURVE('',#1615,#1616,#17,.T.) ;
#1984 = EDGE_CURVE('',#1616,#1617,#28,.T.) ;
#1985 = EDGE_CURVE('',#1617,#1612,#110,.T.) ;
#1986 = EDGE_CURVE('',#1610,#1618,#111,.T.) ;
#1987 = EDGE_CURVE('',#1618,#1619,#112,.T.) ;
#1988 = EDGE_CURVE('',#1619,#1620,#113,.T.) ;
#1989 = EDGE_CURVE('',#1621,#1620,#18,.T.) ;
#1990 = EDGE_CURVE('',#1621,#1611,#114,.T.) ;
#1991 = EDGE_CURVE('',#1615,#1621,#559,.T.) ;
#1992 = EDGE_CURVE('',#1616,#1620,#560,.T.) ;
#1993 = EDGE_CURVE('',#1612,#1619,#561,.T.) ;
#1994 = EDGE_CURVE('',#1546,#1613,#115,.T.) ;
#1995 = EDGE_CURVE('',#1618,#1547,#116,.T.) ;
#1996 = EDGE_CURVE('',#1622,#1623,#562,.T.) ;
#1997 = EDGE_CURVE('',#1622,#1561,#117,.T.) ;
#1998 = EDGE_CURVE('',#1565,#1624,#118,.T.) ;
#1999 = EDGE_CURVE('',#1625,#1624,#563,.T.) ;
#2000 = EDGE_CURVE('',#1623,#1625,#1332,.T.) ;
#2001 = EDGE_CURVE('',#1626,#1627,#119,.T.) ;
#2002 = EDGE_CURVE('',#1627,#1622,#120,.T.) ;
#2003 = EDGE_CURVE('',#1623,#1628,#121,.T.) ;
#2004 = EDGE_CURVE('',#1628,#1629,#29,.T.) ;
#2005 = EDGE_CURVE('',#1629,#1630,#19,.T.) ;
#2006 = EDGE_CURVE('',#1630,#1631,#30,.T.) ;
#2007 = EDGE_CURVE('',#1631,#1626,#122,.T.) ;
#2008 = EDGE_CURVE('',#1624,#1632,#123,.T.) ;
#2009 = EDGE_CURVE('',#1632,#1633,#124,.T.) ;
#2010 = EDGE_CURVE('',#1633,#1634,#125,.T.) ;
#2011 = EDGE_CURVE('',#1635,#1634,#20,.T.) ;
#2012 = EDGE_CURVE('',#1635,#1625,#126,.T.) ;
#2013 = EDGE_CURVE('',#1629,#1635,#564,.T.) ;
#2014 = EDGE_CURVE('',#1630,#1634,#565,.T.) ;
#2015 = EDGE_CURVE('',#1626,#1633,#566,.T.) ;
#2016 = EDGE_CURVE('',#1563,#1627,#127,.T.) ;
#2017 = EDGE_CURVE('',#1632,#1564,#128,.T.) ;
#2018 = EDGE_CURVE('',#1636,#1636,#1333,.T.) ;
#2019 = EDGE_CURVE('',#1636,#1637,#567,.T.) ;
#2020 = EDGE_CURVE('',#1637,#1637,#1334,.T.) ;
#2021 = EDGE_CURVE('',#1638,#1638,#1335,.T.) ;
#2022 = EDGE_CURVE('',#1638,#1639,#568,.T.) ;
#2023 = EDGE_CURVE('',#1639,#1639,#1336,.T.) ;
#2024 = EDGE_CURVE('',#1640,#1641,#569,.T.) ;
#2025 = EDGE_CURVE('',#1641,#1642,#570,.T.) ;
#2026 = EDGE_CURVE('',#1643,#1642,#571,.T.) ;
#2027 = EDGE_CURVE('',#1643,#1640,#572,.T.) ;
#2028 = EDGE_CURVE('',#1644,#1645,#573,.T.) ;
#2029 = EDGE_CURVE('',#1645,#1646,#574,.T.) ;
#2030 = EDGE_CURVE('',#1647,#1646,#575,.T.) ;
#2031 = EDGE_CURVE('',#1647,#1644,#576,.T.) ;
#2032 = EDGE_CURVE('',#1648,#1649,#577,.T.) ;
#2033 = EDGE_CURVE('',#1648,#1650,#578,.T.) ;
#2034 = EDGE_CURVE('',#1650,#1651,#579,.T.) ;
#2035 = EDGE_CURVE('',#1651,#1649,#580,.T.) ;
#2036 = EDGE_CURVE('',#1652,#1653,#581,.T.) ;
#2037 = EDGE_CURVE('',#1653,#1654,#582,.T.) ;
#2038 = EDGE_CURVE('',#1655,#1654,#583,.T.) ;
#2039 = EDGE_CURVE('',#1655,#1652,#584,.T.) ;
#2040 = EDGE_CURVE('',#1646,#1648,#1337,.T.) ;
#2041 = EDGE_CURVE('',#1649,#1655,#1338,.T.) ;
#2042 = EDGE_CURVE('',#1654,#1643,#1339,.T.) ;
#2043 = EDGE_CURVE('',#1642,#1647,#1340,.T.) ;
#2044 = EDGE_CURVE('',#1650,#1645,#1341,.T.) ;
#2045 = EDGE_CURVE('',#1644,#1641,#1342,.T.) ;
#2046 = EDGE_CURVE('',#1640,#1653,#1343,.T.) ;
#2047 = EDGE_CURVE('',#1652,#1651,#1344,.T.) ;
#2048 = EDGE_CURVE('',#1656,#1656,#1345,.T.) ;
#2049 = EDGE_CURVE('',#1656,#1657,#585,.T.) ;
#2050 = EDGE_CURVE('',#1657,#1657,#1346,.T.) ;
#2051 = EDGE_CURVE('',#1658,#1659,#586,.T.) ;
#2052 = EDGE_CURVE('',#1658,#1660,#587,.T.) ;
#2053 = EDGE_CURVE('',#1661,#1660,#588,.T.) ;
#2054 = EDGE_CURVE('',#1661,#1662,#589,.T.) ;
#2055 = EDGE_CURVE('',#1663,#1662,#590,.T.) ;
#2056 = EDGE_CURVE('',#1663,#1664,#591,.T.) ;
#2057 = EDGE_CURVE('',#1665,#1664,#592,.T.) ;
#2058 = EDGE_CURVE('',#1665,#1659,#593,.T.) ;
#2059 = EDGE_CURVE('',#1666,#1667,#594,.T.) ;
#2060 = EDGE_CURVE('',#1667,#1668,#595,.T.) ;
#2061 = EDGE_CURVE('',#1668,#1669,#596,.T.) ;
#2062 = EDGE_CURVE('',#1669,#1670,#597,.T.) ;
#2063 = EDGE_CURVE('',#1670,#1671,#598,.T.) ;
#2064 = EDGE_CURVE('',#1671,#1672,#599,.T.) ;
#2065 = EDGE_CURVE('',#1672,#1673,#600,.T.) ;
#2066 = EDGE_CURVE('',#1673,#1666,#601,.T.) ;
#2067 = EDGE_CURVE('',#1668,#1658,#602,.T.) ;
#2068 = EDGE_CURVE('',#1660,#1667,#603,.T.) ;
#2069 = EDGE_CURVE('',#1666,#1661,#604,.T.) ;
#2070 = EDGE_CURVE('',#1662,#1673,#605,.T.) ;
#2071 = EDGE_CURVE('',#1672,#1663,#606,.T.) ;
#2072 = EDGE_CURVE('',#1664,#1671,#607,.T.) ;
#2073 = EDGE_CURVE('',#1670,#1665,#608,.T.) ;
#2074 = EDGE_CURVE('',#1659,#1669,#609,.T.) ;
#2075 = EDGE_CURVE('',#1674,#1675,#610,.T.) ;
#2076 = EDGE_CURVE('',#1664,#1674,#1347,.T.) ;
#2077 = EDGE_CURVE('',#1671,#1675,#1348,.T.) ;
#2078 = EDGE_CURVE('',#1676,#1665,#1349,.T.) ;
#2079 = EDGE_CURVE('',#1676,#1677,#611,.T.) ;
#2080 = EDGE_CURVE('',#1677,#1670,#1350,.T.) ;
#2081 = EDGE_CURVE('',#1677,#1675,#612,.T.) ;
#2082 = EDGE_CURVE('',#1674,#1676,#613,.T.) ;
#2083 = EDGE_CURVE('',#1676,#1678,#614,.T.) ;
#2084 = EDGE_CURVE('',#1679,#1678,#615,.T.) ;
#2085 = EDGE_CURVE('',#1677,#1679,#616,.T.) ;
#2086 = EDGE_CURVE('',#1680,#1675,#617,.T.) ;
#2087 = EDGE_CURVE('',#1680,#1681,#618,.T.) ;
#2088 = EDGE_CURVE('',#1681,#1674,#619,.T.) ;
#2089 = EDGE_CURVE('',#1679,#1680,#620,.T.) ;
#2090 = EDGE_CURVE('',#1678,#1681,#621,.T.) ;
#2091 = EDGE_CURVE('',#1682,#1683,#622,.T.) ;
#2092 = EDGE_CURVE('',#1659,#1682,#1351,.T.) ;
#2093 = EDGE_CURVE('',#1669,#1683,#1352,.T.) ;
#2094 = EDGE_CURVE('',#1684,#1658,#1353,.T.) ;
#2095 = EDGE_CURVE('',#1684,#1685,#623,.T.) ;
#2096 = EDGE_CURVE('',#1685,#1668,#1354,.T.) ;
#2097 = EDGE_CURVE('',#1685,#1683,#624,.T.) ;
#2098 = EDGE_CURVE('',#1682,#1684,#625,.T.) ;
#2099 = EDGE_CURVE('',#1684,#1686,#626,.T.) ;
#2100 = EDGE_CURVE('',#1687,#1686,#627,.T.) ;
#2101 = EDGE_CURVE('',#1685,#1687,#628,.T.) ;
#2102 = EDGE_CURVE('',#1688,#1683,#629,.T.) ;
#2103 = EDGE_CURVE('',#1688,#1689,#630,.T.) ;
#2104 = EDGE_CURVE('',#1689,#1682,#631,.T.) ;
#2105 = EDGE_CURVE('',#1687,#1688,#632,.T.) ;
#2106 = EDGE_CURVE('',#1686,#1689,#633,.T.) ;
#2107 = EDGE_CURVE('',#1690,#1691,#634,.T.) ;
#2108 = EDGE_CURVE('',#1660,#1690,#1355,.T.) ;
#2109 = EDGE_CURVE('',#1667,#1691,#1356,.T.) ;
#2110 = EDGE_CURVE('',#1692,#1661,#1357,.T.) ;
#2111 = EDGE_CURVE('',#1692,#1693,#635,.T.) ;
#2112 = EDGE_CURVE('',#1693,#1666,#1358,.T.) ;
#2113 = EDGE_CURVE('',#1693,#1691,#636,.T.) ;
#2114 = EDGE_CURVE('',#1690,#1692,#637,.T.) ;
#2115 = EDGE_CURVE('',#1692,#1694,#638,.T.) ;
#2116 = EDGE_CURVE('',#1695,#1694,#639,.T.) ;
#2117 = EDGE_CURVE('',#1693,#1695,#640,.T.) ;
#2118 = EDGE_CURVE('',#1696,#1691,#641,.T.) ;
#2119 = EDGE_CURVE('',#1696,#1697,#642,.T.) ;
#2120 = EDGE_CURVE('',#1697,#1690,#643,.T.) ;
#2121 = EDGE_CURVE('',#1695,#1696,#644,.T.) ;
#2122 = EDGE_CURVE('',#1694,#1697,#645,.T.) ;
#2123 = EDGE_CURVE('',#1698,#1699,#646,.T.) ;
#2124 = EDGE_CURVE('',#1662,#1698,#1359,.T.) ;
#2125 = EDGE_CURVE('',#1673,#1699,#1360,.T.) ;
#2126 = EDGE_CURVE('',#1700,#1663,#1361,.T.) ;
#2127 = EDGE_CURVE('',#1700,#1701,#647,.T.) ;
#2128 = EDGE_CURVE('',#1701,#1672,#1362,.T.) ;
#2129 = EDGE_CURVE('',#1701,#1699,#648,.T.) ;
#2130 = EDGE_CURVE('',#1698,#1700,#649,.T.) ;
#2131 = EDGE_CURVE('',#1700,#1702,#650,.T.) ;
#2132 = EDGE_CURVE('',#1703,#1702,#651,.T.) ;
#2133 = EDGE_CURVE('',#1701,#1703,#652,.T.) ;
#2134 = EDGE_CURVE('',#1704,#1699,#653,.T.) ;
#2135 = EDGE_CURVE('',#1704,#1705,#654,.T.) ;
#2136 = EDGE_CURVE('',#1705,#1698,#655,.T.) ;
#2137 = EDGE_CURVE('',#1703,#1704,#656,.T.) ;
#2138 = EDGE_CURVE('',#1702,#1705,#657,.T.) ;
#2139 = EDGE_CURVE('',#1706,#1706,#1363,.T.) ;
#2140 = EDGE_CURVE('',#1706,#1707,#1364,.T.) ;
#2141 = EDGE_CURVE('',#1707,#1708,#1365,.T.) ;
#2142 = EDGE_CURVE('',#1708,#1707,#1366,.T.) ;
#2143 = EDGE_CURVE('',#1709,#1709,#1367,.T.) ;
#2144 = EDGE_CURVE('',#1709,#1710,#1368,.T.) ;
#2145 = EDGE_CURVE('',#1710,#1710,#1369,.T.) ;
#2146 = EDGE_CURVE('',#1711,#1712,#1370,.T.) ;
#2147 = EDGE_CURVE('',#1712,#1711,#1371,.T.) ;
#2148 = EDGE_CURVE('',#1712,#1713,#1372,.T.) ;
#2149 = EDGE_CURVE('',#1713,#1714,#1373,.T.) ;
#2150 = EDGE_CURVE('',#1714,#1713,#1374,.T.) ;
#2151 = EDGE_CURVE('',#1715,#1716,#1375,.T.) ;
#2152 = EDGE_CURVE('',#1716,#1717,#1376,.T.) ;
#2153 = EDGE_CURVE('',#1718,#1717,#1377,.T.) ;
#2154 = EDGE_CURVE('',#1717,#1718,#1378,.T.) ;
#2155 = EDGE_CURVE('',#1716,#1715,#1379,.T.) ;
#2156 = EDGE_CURVE('',#1719,#1720,#1380,.T.) ;
#2157 = EDGE_CURVE('',#1720,#1719,#1381,.T.) ;
#2158 = EDGE_CURVE('',#1720,#1721,#1382,.T.) ;
#2159 = EDGE_CURVE('',#1721,#1722,#1383,.T.) ;
#2160 = EDGE_CURVE('',#1722,#1721,#1384,.T.) ;
#2161 = EDGE_CURVE('',#1723,#1724,#1385,.T.) ;
#2162 = EDGE_CURVE('',#1724,#1723,#1386,.T.) ;
#2163 = EDGE_CURVE('',#1724,#1725,#1387,.T.) ;
#2164 = EDGE_CURVE('',#1725,#1725,#1388,.T.) ;
#2165 = EDGE_CURVE('',#1726,#1726,#1389,.T.) ;
#2166 = EDGE_CURVE('',#1726,#1727,#1390,.T.) ;
#2167 = EDGE_CURVE('',#1727,#1727,#1391,.T.) ;
#2168 = EDGE_CURVE('',#1728,#1729,#1392,.T.) ;
#2169 = EDGE_CURVE('',#1729,#1728,#1393,.T.) ;
#2170 = EDGE_CURVE('',#1729,#1730,#1394,.T.) ;
#2171 = EDGE_CURVE('',#1730,#1731,#1395,.T.) ;
#2172 = EDGE_CURVE('',#1731,#1730,#1396,.T.) ;
#2173 = EDGE_CURVE('',#1719,#1708,#658,.T.) ;
#2174 = EDGE_CURVE('',#1706,#1710,#659,.T.) ;
#2175 = EDGE_CURVE('',#1709,#1714,#660,.T.) ;
#2176 = EDGE_CURVE('',#1711,#1715,#661,.T.) ;
#2177 = EDGE_CURVE('',#1722,#1723,#662,.T.) ;
#2178 = EDGE_CURVE('',#1725,#1726,#663,.T.) ;
#2179 = EDGE_CURVE('',#1727,#1728,#664,.T.) ;
#2180 = EDGE_CURVE('',#1731,#1718,#665,.T.) ;
#2181 = EDGE_CURVE('',#1732,#1732,#1397,.T.) ;
#2182 = EDGE_CURVE('',#1732,#1733,#1398,.T.) ;
#2183 = EDGE_CURVE('',#1733,#1734,#1399,.T.) ;
#2184 = EDGE_CURVE('',#1734,#1733,#1400,.T.) ;
#2185 = EDGE_CURVE('',#1735,#1735,#1401,.T.) ;
#2186 = EDGE_CURVE('',#1735,#1736,#1402,.T.) ;
#2187 = EDGE_CURVE('',#1736,#1736,#1403,.T.) ;
#2188 = EDGE_CURVE('',#1737,#1738,#1404,.T.) ;
#2189 = EDGE_CURVE('',#1738,#1737,#1405,.T.) ;
#2190 = EDGE_CURVE('',#1738,#1739,#1406,.T.) ;
#2191 = EDGE_CURVE('',#1739,#1740,#1407,.T.) ;
#2192 = EDGE_CURVE('',#1740,#1739,#1408,.T.) ;
#2193 = EDGE_CURVE('',#1741,#1742,#1409,.T.) ;
#2194 = EDGE_CURVE('',#1742,#1743,#1410,.T.) ;
#2195 = EDGE_CURVE('',#1744,#1743,#1411,.T.) ;
#2196 = EDGE_CURVE('',#1743,#1744,#1412,.T.) ;
#2197 = EDGE_CURVE('',#1742,#1741,#1413,.T.) ;
#2198 = EDGE_CURVE('',#1745,#1746,#1414,.T.) ;
#2199 = EDGE_CURVE('',#1746,#1745,#1415,.T.) ;
#2200 = EDGE_CURVE('',#1746,#1747,#1416,.T.) ;
#2201 = EDGE_CURVE('',#1747,#1748,#1417,.T.) ;
#2202 = EDGE_CURVE('',#1748,#1747,#1418,.T.) ;
#2203 = EDGE_CURVE('',#1749,#1750,#1419,.T.) ;
#2204 = EDGE_CURVE('',#1750,#1749,#1420,.T.) ;
#2205 = EDGE_CURVE('',#1750,#1751,#1421,.T.) ;
#2206 = EDGE_CURVE('',#1751,#1751,#1422,.T.) ;
#2207 = EDGE_CURVE('',#1752,#1752,#1423,.T.) ;
#2208 = EDGE_CURVE('',#1752,#1753,#1424,.T.) ;
#2209 = EDGE_CURVE('',#1753,#1753,#1425,.T.) ;
#2210 = EDGE_CURVE('',#1754,#1755,#1426,.T.) ;
#2211 = EDGE_CURVE('',#1755,#1754,#1427,.T.) ;
#2212 = EDGE_CURVE('',#1755,#1756,#1428,.T.) ;
#2213 = EDGE_CURVE('',#1756,#1757,#1429,.T.) ;
#2214 = EDGE_CURVE('',#1757,#1756,#1430,.T.) ;
#2215 = EDGE_CURVE('',#1745,#1734,#666,.T.) ;
#2216 = EDGE_CURVE('',#1732,#1736,#667,.T.) ;
#2217 = EDGE_CURVE('',#1735,#1740,#668,.T.) ;
#2218 = EDGE_CURVE('',#1737,#1741,#669,.T.) ;
#2219 = EDGE_CURVE('',#1748,#1749,#670,.T.) ;
#2220 = EDGE_CURVE('',#1751,#1752,#671,.T.) ;
#2221 = EDGE_CURVE('',#1753,#1754,#672,.T.) ;
#2222 = EDGE_CURVE('',#1757,#1744,#673,.T.) ;
#2223 = EDGE_CURVE('',#1758,#1758,#1431,.T.) ;
#2224 = EDGE_CURVE('',#1758,#1759,#1432,.T.) ;
#2225 = EDGE_CURVE('',#1759,#1760,#1433,.T.) ;
#2226 = EDGE_CURVE('',#1760,#1759,#1434,.T.) ;
#2227 = EDGE_CURVE('',#1761,#1761,#1435,.T.) ;
#2228 = EDGE_CURVE('',#1761,#1762,#1436,.T.) ;
#2229 = EDGE_CURVE('',#1762,#1762,#1437,.T.) ;
#2230 = EDGE_CURVE('',#1763,#1764,#1438,.T.) ;
#2231 = EDGE_CURVE('',#1764,#1763,#1439,.T.) ;
#2232 = EDGE_CURVE('',#1764,#1765,#1440,.T.) ;
#2233 = EDGE_CURVE('',#1765,#1766,#1441,.T.) ;
#2234 = EDGE_CURVE('',#1766,#1765,#1442,.T.) ;
#2235 = EDGE_CURVE('',#1767,#1768,#1443,.T.) ;
#2236 = EDGE_CURVE('',#1768,#1769,#1444,.T.) ;
#2237 = EDGE_CURVE('',#1770,#1769,#1445,.T.) ;
#2238 = EDGE_CURVE('',#1769,#1770,#1446,.T.) ;
#2239 = EDGE_CURVE('',#1768,#1767,#1447,.T.) ;
#2240 = EDGE_CURVE('',#1771,#1772,#1448,.T.) ;
#2241 = EDGE_CURVE('',#1772,#1771,#1449,.T.) ;
#2242 = EDGE_CURVE('',#1772,#1773,#1450,.T.) ;
#2243 = EDGE_CURVE('',#1773,#1774,#1451,.T.) ;
#2244 = EDGE_CURVE('',#1774,#1773,#1452,.T.) ;
#2245 = EDGE_CURVE('',#1775,#1776,#1453,.T.) ;
#2246 = EDGE_CURVE('',#1776,#1775,#1454,.T.) ;
#2247 = EDGE_CURVE('',#1776,#1777,#1455,.T.) ;
#2248 = EDGE_CURVE('',#1777,#1777,#1456,.T.) ;
#2249 = EDGE_CURVE('',#1778,#1778,#1457,.T.) ;
#2250 = EDGE_CURVE('',#1778,#1779,#1458,.T.) ;
#2251 = EDGE_CURVE('',#1779,#1779,#1459,.T.) ;
#2252 = EDGE_CURVE('',#1780,#1781,#1460,.T.) ;
#2253 = EDGE_CURVE('',#1781,#1780,#1461,.T.) ;
#2254 = EDGE_CURVE('',#1781,#1782,#1462,.T.) ;
#2255 = EDGE_CURVE('',#1782,#1783,#1463,.T.) ;
#2256 = EDGE_CURVE('',#1783,#1782,#1464,.T.) ;
#2257 = EDGE_CURVE('',#1771,#1760,#674,.T.) ;
#2258 = EDGE_CURVE('',#1758,#1762,#675,.T.) ;
#2259 = EDGE_CURVE('',#1761,#1766,#676,.T.) ;
#2260 = EDGE_CURVE('',#1763,#1767,#677,.T.) ;
#2261 = EDGE_CURVE('',#1774,#1775,#678,.T.) ;
#2262 = EDGE_CURVE('',#1777,#1778,#679,.T.) ;
#2263 = EDGE_CURVE('',#1779,#1780,#680,.T.) ;
#2264 = EDGE_CURVE('',#1783,#1770,#681,.T.) ;
#2265 = EDGE_CURVE('',#1784,#1784,#1465,.T.) ;
#2266 = EDGE_CURVE('',#1784,#1785,#1466,.T.) ;
#2267 = EDGE_CURVE('',#1785,#1786,#1467,.T.) ;
#2268 = EDGE_CURVE('',#1786,#1785,#1468,.T.) ;
#2269 = EDGE_CURVE('',#1787,#1787,#1469,.T.) ;
#2270 = EDGE_CURVE('',#1787,#1788,#1470,.T.) ;
#2271 = EDGE_CURVE('',#1788,#1788,#1471,.T.) ;
#2272 = EDGE_CURVE('',#1789,#1790,#1472,.T.) ;
#2273 = EDGE_CURVE('',#1790,#1789,#1473,.T.) ;
#2274 = EDGE_CURVE('',#1790,#1791,#1474,.T.) ;
#2275 = EDGE_CURVE('',#1791,#1792,#1475,.T.) ;
#2276 = EDGE_CURVE('',#1792,#1791,#1476,.T.) ;
#2277 = EDGE_CURVE('',#1793,#1794,#1477,.T.) ;
#2278 = EDGE_CURVE('',#1794,#1795,#1478,.T.) ;
#2279 = EDGE_CURVE('',#1796,#1795,#1479,.T.) ;
#2280 = EDGE_CURVE('',#1795,#1796,#1480,.T.) ;
#2281 = EDGE_CURVE('',#1794,#1793,#1481,.T.) ;
#2282 = EDGE_CURVE('',#1797,#1798,#1482,.T.) ;
#2283 = EDGE_CURVE('',#1798,#1797,#1483,.T.) ;
#2284 = EDGE_CURVE('',#1798,#1799,#1484,.T.) ;
#2285 = EDGE_CURVE('',#1799,#1800,#1485,.T.) ;
#2286 = EDGE_CURVE('',#1800,#1799,#1486,.T.) ;
#2287 = EDGE_CURVE('',#1801,#1802,#1487,.T.) ;
#2288 = EDGE_CURVE('',#1802,#1801,#1488,.T.) ;
#2289 = EDGE_CURVE('',#1802,#1803,#1489,.T.) ;
#2290 = EDGE_CURVE('',#1803,#1803,#1490,.T.) ;
#2291 = EDGE_CURVE('',#1804,#1804,#1491,.T.) ;
#2292 = EDGE_CURVE('',#1804,#1805,#1492,.T.) ;
#2293 = EDGE_CURVE('',#1805,#1805,#1493,.T.) ;
#2294 = EDGE_CURVE('',#1806,#1807,#1494,.T.) ;
#2295 = EDGE_CURVE('',#1807,#1806,#1495,.T.) ;
#2296 = EDGE_CURVE('',#1807,#1808,#1496,.T.) ;
#2297 = EDGE_CURVE('',#1808,#1809,#1497,.T.) ;
#2298 = EDGE_CURVE('',#1809,#1808,#1498,.T.) ;
#2299 = EDGE_CURVE('',#1797,#1786,#682,.T.) ;
#2300 = EDGE_CURVE('',#1784,#1788,#683,.T.) ;
#2301 = EDGE_CURVE('',#1787,#1792,#684,.T.) ;
#2302 = EDGE_CURVE('',#1789,#1793,#685,.T.) ;
#2303 = EDGE_CURVE('',#1800,#1801,#686,.T.) ;
#2304 = EDGE_CURVE('',#1803,#1804,#687,.T.) ;
#2305 = EDGE_CURVE('',#1805,#1806,#688,.T.) ;
#2306 = EDGE_CURVE('',#1809,#1796,#689,.T.) ;
#2307 = ORIENTED_EDGE('',*,*,#1810,.F.) ;
#2308 = ORIENTED_EDGE('',*,*,#1811,.F.) ;
#2309 = ORIENTED_EDGE('',*,*,#1812,.T.) ;
#2310 = ORIENTED_EDGE('',*,*,#1813,.T.) ;
#2311 = ORIENTED_EDGE('',*,*,#1812,.F.) ;
#2312 = ORIENTED_EDGE('',*,*,#1814,.F.) ;
#2313 = ORIENTED_EDGE('',*,*,#1815,.T.) ;
#2314 = ORIENTED_EDGE('',*,*,#1816,.T.) ;
#2315 = ORIENTED_EDGE('',*,*,#1817,.T.) ;
#2316 = ORIENTED_EDGE('',*,*,#1815,.F.) ;
#2317 = ORIENTED_EDGE('',*,*,#1810,.T.) ;
#2318 = ORIENTED_EDGE('',*,*,#1811,.T.) ;
#2319 = ORIENTED_EDGE('',*,*,#1818,.T.) ;
#2320 = ORIENTED_EDGE('',*,*,#1816,.F.) ;
#2321 = ORIENTED_EDGE('',*,*,#1817,.F.) ;
#2322 = ORIENTED_EDGE('',*,*,#1818,.F.) ;
#2323 = ORIENTED_EDGE('',*,*,#1813,.F.) ;
#2324 = ORIENTED_EDGE('',*,*,#1814,.T.) ;
#2325 = ORIENTED_EDGE('',*,*,#1819,.F.) ;
#2326 = ORIENTED_EDGE('',*,*,#1820,.F.) ;
#2327 = ORIENTED_EDGE('',*,*,#1821,.T.) ;
#2328 = ORIENTED_EDGE('',*,*,#1822,.T.) ;
#2329 = ORIENTED_EDGE('',*,*,#1823,.T.) ;
#2330 = ORIENTED_EDGE('',*,*,#1821,.F.) ;
#2331 = ORIENTED_EDGE('',*,*,#1819,.T.) ;
#2332 = ORIENTED_EDGE('',*,*,#1820,.T.) ;
#2333 = ORIENTED_EDGE('',*,*,#1824,.T.) ;
#2334 = ORIENTED_EDGE('',*,*,#1825,.F.) ;
#2335 = ORIENTED_EDGE('',*,*,#1826,.F.) ;
#2336 = ORIENTED_EDGE('',*,*,#1824,.F.) ;
#2337 = ORIENTED_EDGE('',*,*,#1827,.F.) ;
#2338 = ORIENTED_EDGE('',*,*,#1828,.F.) ;
#2339 = ORIENTED_EDGE('',*,*,#1829,.T.) ;
#2340 = ORIENTED_EDGE('',*,*,#1825,.T.) ;
#2341 = ORIENTED_EDGE('',*,*,#1826,.T.) ;
#2342 = ORIENTED_EDGE('',*,*,#1829,.F.) ;
#2343 = ORIENTED_EDGE('',*,*,#1827,.T.) ;
#2344 = ORIENTED_EDGE('',*,*,#1828,.T.) ;
#2345 = ORIENTED_EDGE('',*,*,#1830,.T.) ;
#2346 = ORIENTED_EDGE('',*,*,#1822,.F.) ;
#2347 = ORIENTED_EDGE('',*,*,#1823,.F.) ;
#2348 = ORIENTED_EDGE('',*,*,#1830,.F.) ;
#2349 = ORIENTED_EDGE('',*,*,#1831,.F.) ;
#2350 = ORIENTED_EDGE('',*,*,#1832,.T.) ;
#2351 = ORIENTED_EDGE('',*,*,#1831,.T.) ;
#2352 = ORIENTED_EDGE('',*,*,#1832,.F.) ;
#2353 = ORIENTED_EDGE('',*,*,#1833,.F.) ;
#2354 = ORIENTED_EDGE('',*,*,#1834,.T.) ;
#2355 = ORIENTED_EDGE('',*,*,#1833,.T.) ;
#2356 = ORIENTED_EDGE('',*,*,#1834,.F.) ;
#2357 = ORIENTED_EDGE('',*,*,#1835,.F.) ;
#2358 = ORIENTED_EDGE('',*,*,#1836,.T.) ;
#2359 = ORIENTED_EDGE('',*,*,#1835,.T.) ;
#2360 = ORIENTED_EDGE('',*,*,#1836,.F.) ;
#2361 = ORIENTED_EDGE('',*,*,#1837,.F.) ;
#2362 = ORIENTED_EDGE('',*,*,#1838,.T.) ;
#2363 = ORIENTED_EDGE('',*,*,#1837,.T.) ;
#2364 = ORIENTED_EDGE('',*,*,#1838,.F.) ;
#2365 = ORIENTED_EDGE('',*,*,#1839,.F.) ;
#2366 = ORIENTED_EDGE('',*,*,#1840,.T.) ;
#2367 = ORIENTED_EDGE('',*,*,#1839,.T.) ;
#2368 = ORIENTED_EDGE('',*,*,#1840,.F.) ;
#2369 = ORIENTED_EDGE('',*,*,#1841,.F.) ;
#2370 = ORIENTED_EDGE('',*,*,#1842,.T.) ;
#2371 = ORIENTED_EDGE('',*,*,#1841,.T.) ;
#2372 = ORIENTED_EDGE('',*,*,#1842,.F.) ;
#2373 = ORIENTED_EDGE('',*,*,#1843,.F.) ;
#2374 = ORIENTED_EDGE('',*,*,#1844,.T.) ;
#2375 = ORIENTED_EDGE('',*,*,#1843,.T.) ;
#2376 = ORIENTED_EDGE('',*,*,#1844,.F.) ;
#2377 = ORIENTED_EDGE('',*,*,#1845,.F.) ;
#2378 = ORIENTED_EDGE('',*,*,#1846,.T.) ;
#2379 = ORIENTED_EDGE('',*,*,#1845,.T.) ;
#2380 = ORIENTED_EDGE('',*,*,#1846,.F.) ;
#2381 = ORIENTED_EDGE('',*,*,#1847,.F.) ;
#2382 = ORIENTED_EDGE('',*,*,#1848,.T.) ;
#2383 = ORIENTED_EDGE('',*,*,#1847,.T.) ;
#2384 = ORIENTED_EDGE('',*,*,#1848,.F.) ;
#2385 = ORIENTED_EDGE('',*,*,#1849,.F.) ;
#2386 = ORIENTED_EDGE('',*,*,#1850,.T.) ;
#2387 = ORIENTED_EDGE('',*,*,#1849,.T.) ;
#2388 = ORIENTED_EDGE('',*,*,#1850,.F.) ;
#2389 = ORIENTED_EDGE('',*,*,#1851,.F.) ;
#2390 = ORIENTED_EDGE('',*,*,#1852,.T.) ;
#2391 = ORIENTED_EDGE('',*,*,#1851,.T.) ;
#2392 = ORIENTED_EDGE('',*,*,#1852,.F.) ;
#2393 = ORIENTED_EDGE('',*,*,#1853,.F.) ;
#2394 = ORIENTED_EDGE('',*,*,#1854,.T.) ;
#2395 = ORIENTED_EDGE('',*,*,#1853,.T.) ;
#2396 = ORIENTED_EDGE('',*,*,#1854,.F.) ;
#2397 = ORIENTED_EDGE('',*,*,#1855,.F.) ;
#2398 = ORIENTED_EDGE('',*,*,#1856,.T.) ;
#2399 = ORIENTED_EDGE('',*,*,#1855,.T.) ;
#2400 = ORIENTED_EDGE('',*,*,#1856,.F.) ;
#2401 = ORIENTED_EDGE('',*,*,#1857,.F.) ;
#2402 = ORIENTED_EDGE('',*,*,#1858,.T.) ;
#2403 = ORIENTED_EDGE('',*,*,#1857,.T.) ;
#2404 = ORIENTED_EDGE('',*,*,#1858,.F.) ;
#2405 = ORIENTED_EDGE('',*,*,#1859,.F.) ;
#2406 = ORIENTED_EDGE('',*,*,#1860,.T.) ;
#2407 = ORIENTED_EDGE('',*,*,#1859,.T.) ;
#2408 = ORIENTED_EDGE('',*,*,#1860,.F.) ;
#2409 = ORIENTED_EDGE('',*,*,#1861,.F.) ;
#2410 = ORIENTED_EDGE('',*,*,#1862,.T.) ;
#2411 = ORIENTED_EDGE('',*,*,#1861,.T.) ;
#2412 = ORIENTED_EDGE('',*,*,#1862,.F.) ;
#2413 = ORIENTED_EDGE('',*,*,#1863,.F.) ;
#2414 = ORIENTED_EDGE('',*,*,#1864,.T.) ;
#2415 = ORIENTED_EDGE('',*,*,#1863,.T.) ;
#2416 = ORIENTED_EDGE('',*,*,#1864,.F.) ;
#2417 = ORIENTED_EDGE('',*,*,#1865,.F.) ;
#2418 = ORIENTED_EDGE('',*,*,#1866,.T.) ;
#2419 = ORIENTED_EDGE('',*,*,#1865,.T.) ;
#2420 = ORIENTED_EDGE('',*,*,#1866,.F.) ;
#2421 = ORIENTED_EDGE('',*,*,#1867,.F.) ;
#2422 = ORIENTED_EDGE('',*,*,#1868,.T.) ;
#2423 = ORIENTED_EDGE('',*,*,#1867,.T.) ;
#2424 = ORIENTED_EDGE('',*,*,#1868,.F.) ;
#2425 = ORIENTED_EDGE('',*,*,#1869,.F.) ;
#2426 = ORIENTED_EDGE('',*,*,#1870,.T.) ;
#2427 = ORIENTED_EDGE('',*,*,#1869,.T.) ;
#2428 = ORIENTED_EDGE('',*,*,#1870,.F.) ;
#2429 = ORIENTED_EDGE('',*,*,#1871,.F.) ;
#2430 = ORIENTED_EDGE('',*,*,#1872,.T.) ;
#2431 = ORIENTED_EDGE('',*,*,#1871,.T.) ;
#2432 = ORIENTED_EDGE('',*,*,#1872,.F.) ;
#2433 = ORIENTED_EDGE('',*,*,#1873,.F.) ;
#2434 = ORIENTED_EDGE('',*,*,#1874,.T.) ;
#2435 = ORIENTED_EDGE('',*,*,#1873,.T.) ;
#2436 = ORIENTED_EDGE('',*,*,#1874,.F.) ;
#2437 = ORIENTED_EDGE('',*,*,#1875,.F.) ;
#2438 = ORIENTED_EDGE('',*,*,#1876,.T.) ;
#2439 = ORIENTED_EDGE('',*,*,#1877,.T.) ;
#2440 = ORIENTED_EDGE('',*,*,#1878,.F.) ;
#2441 = ORIENTED_EDGE('',*,*,#1879,.T.) ;
#2442 = ORIENTED_EDGE('',*,*,#1880,.T.) ;
#2443 = ORIENTED_EDGE('',*,*,#1879,.F.) ;
#2444 = ORIENTED_EDGE('',*,*,#1881,.F.) ;
#2445 = ORIENTED_EDGE('',*,*,#1882,.T.) ;
#2446 = ORIENTED_EDGE('',*,*,#1883,.T.) ;
#2447 = ORIENTED_EDGE('',*,*,#1884,.T.) ;
#2448 = ORIENTED_EDGE('',*,*,#1885,.T.) ;
#2449 = ORIENTED_EDGE('',*,*,#1876,.F.) ;
#2450 = ORIENTED_EDGE('',*,*,#1886,.T.) ;
#2451 = ORIENTED_EDGE('',*,*,#1887,.T.) ;
#2452 = ORIENTED_EDGE('',*,*,#1888,.T.) ;
#2453 = ORIENTED_EDGE('',*,*,#1889,.T.) ;
#2454 = ORIENTED_EDGE('',*,*,#1890,.T.) ;
#2455 = ORIENTED_EDGE('',*,*,#1891,.F.) ;
#2456 = ORIENTED_EDGE('',*,*,#1892,.T.) ;
#2457 = ORIENTED_EDGE('',*,*,#1893,.T.) ;
#2458 = ORIENTED_EDGE('',*,*,#1894,.T.) ;
#2459 = ORIENTED_EDGE('',*,*,#1895,.T.) ;
#2460 = ORIENTED_EDGE('',*,*,#1896,.T.) ;
#2461 = ORIENTED_EDGE('',*,*,#1897,.F.) ;
#2462 = ORIENTED_EDGE('',*,*,#1898,.T.) ;
#2463 = ORIENTED_EDGE('',*,*,#1899,.T.) ;
#2464 = ORIENTED_EDGE('',*,*,#1900,.T.) ;
#2465 = ORIENTED_EDGE('',*,*,#1901,.T.) ;
#2466 = ORIENTED_EDGE('',*,*,#1902,.F.) ;
#2467 = ORIENTED_EDGE('',*,*,#1903,.T.) ;
#2468 = ORIENTED_EDGE('',*,*,#1904,.T.) ;
#2469 = ORIENTED_EDGE('',*,*,#1905,.T.) ;
#2470 = ORIENTED_EDGE('',*,*,#1906,.T.) ;
#2471 = ORIENTED_EDGE('',*,*,#1907,.F.) ;
#2472 = ORIENTED_EDGE('',*,*,#1908,.F.) ;
#2473 = ORIENTED_EDGE('',*,*,#1909,.T.) ;
#2474 = ORIENTED_EDGE('',*,*,#1881,.T.) ;
#2475 = ORIENTED_EDGE('',*,*,#1878,.T.) ;
#2476 = ORIENTED_EDGE('',*,*,#1910,.T.) ;
#2477 = ORIENTED_EDGE('',*,*,#1911,.F.) ;
#2478 = ORIENTED_EDGE('',*,*,#1912,.F.) ;
#2479 = ORIENTED_EDGE('',*,*,#1913,.T.) ;
#2480 = ORIENTED_EDGE('',*,*,#1914,.T.) ;
#2481 = ORIENTED_EDGE('',*,*,#1908,.T.) ;
#2482 = ORIENTED_EDGE('',*,*,#1915,.T.) ;
#2483 = ORIENTED_EDGE('',*,*,#1916,.T.) ;
#2484 = ORIENTED_EDGE('',*,*,#1917,.T.) ;
#2485 = ORIENTED_EDGE('',*,*,#1918,.T.) ;
#2486 = ORIENTED_EDGE('',*,*,#1919,.T.) ;
#2487 = ORIENTED_EDGE('',*,*,#1911,.T.) ;
#2488 = ORIENTED_EDGE('',*,*,#1920,.T.) ;
#2489 = ORIENTED_EDGE('',*,*,#1921,.T.) ;
#2490 = ORIENTED_EDGE('',*,*,#1922,.T.) ;
#2491 = ORIENTED_EDGE('',*,*,#1923,.F.) ;
#2492 = ORIENTED_EDGE('',*,*,#1924,.T.) ;
#2493 = ORIENTED_EDGE('',*,*,#1925,.F.) ;
#2494 = ORIENTED_EDGE('',*,*,#1916,.F.) ;
#2495 = ORIENTED_EDGE('',*,*,#1915,.F.) ;
#2496 = ORIENTED_EDGE('',*,*,#1912,.T.) ;
#2497 = ORIENTED_EDGE('',*,*,#1924,.F.) ;
#2498 = ORIENTED_EDGE('',*,*,#1925,.T.) ;
#2499 = ORIENTED_EDGE('',*,*,#1923,.T.) ;
#2500 = ORIENTED_EDGE('',*,*,#1926,.F.) ;
#2501 = ORIENTED_EDGE('',*,*,#1917,.F.) ;
#2502 = ORIENTED_EDGE('',*,*,#1927,.F.) ;
#2503 = ORIENTED_EDGE('',*,*,#1919,.F.) ;
#2504 = ORIENTED_EDGE('',*,*,#1918,.F.) ;
#2505 = ORIENTED_EDGE('',*,*,#1926,.T.) ;
#2506 = ORIENTED_EDGE('',*,*,#1922,.F.) ;
#2507 = ORIENTED_EDGE('',*,*,#1884,.F.) ;
#2508 = ORIENTED_EDGE('',*,*,#1928,.T.) ;
#2509 = ORIENTED_EDGE('',*,*,#1913,.F.) ;
#2510 = ORIENTED_EDGE('',*,*,#1927,.T.) ;
#2511 = ORIENTED_EDGE('',*,*,#1921,.F.) ;
#2512 = ORIENTED_EDGE('',*,*,#1929,.T.) ;
#2513 = ORIENTED_EDGE('',*,*,#1880,.F.) ;
#2514 = ORIENTED_EDGE('',*,*,#1909,.F.) ;
#2515 = ORIENTED_EDGE('',*,*,#1914,.F.) ;
#2516 = ORIENTED_EDGE('',*,*,#1928,.F.) ;
#2517 = ORIENTED_EDGE('',*,*,#1883,.F.) ;
#2518 = ORIENTED_EDGE('',*,*,#1882,.F.) ;
#2519 = ORIENTED_EDGE('',*,*,#1929,.F.) ;
#2520 = ORIENTED_EDGE('',*,*,#1920,.F.) ;
#2521 = ORIENTED_EDGE('',*,*,#1910,.F.) ;
#2522 = ORIENTED_EDGE('',*,*,#1877,.F.) ;
#2523 = ORIENTED_EDGE('',*,*,#1885,.F.) ;
#2524 = ORIENTED_EDGE('',*,*,#1930,.F.) ;
#2525 = ORIENTED_EDGE('',*,*,#1931,.T.) ;
#2526 = ORIENTED_EDGE('',*,*,#1897,.T.) ;
#2527 = ORIENTED_EDGE('',*,*,#1932,.T.) ;
#2528 = ORIENTED_EDGE('',*,*,#1933,.F.) ;
#2529 = ORIENTED_EDGE('',*,*,#1934,.F.) ;
#2530 = ORIENTED_EDGE('',*,*,#1935,.T.) ;
#2531 = ORIENTED_EDGE('',*,*,#1936,.T.) ;
#2532 = ORIENTED_EDGE('',*,*,#1930,.T.) ;
#2533 = ORIENTED_EDGE('',*,*,#1937,.T.) ;
#2534 = ORIENTED_EDGE('',*,*,#1938,.T.) ;
#2535 = ORIENTED_EDGE('',*,*,#1939,.T.) ;
#2536 = ORIENTED_EDGE('',*,*,#1940,.T.) ;
#2537 = ORIENTED_EDGE('',*,*,#1941,.T.) ;
#2538 = ORIENTED_EDGE('',*,*,#1933,.T.) ;
#2539 = ORIENTED_EDGE('',*,*,#1942,.T.) ;
#2540 = ORIENTED_EDGE('',*,*,#1943,.T.) ;
#2541 = ORIENTED_EDGE('',*,*,#1944,.T.) ;
#2542 = ORIENTED_EDGE('',*,*,#1945,.F.) ;
#2543 = ORIENTED_EDGE('',*,*,#1946,.T.) ;
#2544 = ORIENTED_EDGE('',*,*,#1947,.F.) ;
#2545 = ORIENTED_EDGE('',*,*,#1938,.F.) ;
#2546 = ORIENTED_EDGE('',*,*,#1937,.F.) ;
#2547 = ORIENTED_EDGE('',*,*,#1934,.T.) ;
#2548 = ORIENTED_EDGE('',*,*,#1946,.F.) ;
#2549 = ORIENTED_EDGE('',*,*,#1947,.T.) ;
#2550 = ORIENTED_EDGE('',*,*,#1945,.T.) ;
#2551 = ORIENTED_EDGE('',*,*,#1948,.F.) ;
#2552 = ORIENTED_EDGE('',*,*,#1939,.F.) ;
#2553 = ORIENTED_EDGE('',*,*,#1949,.F.) ;
#2554 = ORIENTED_EDGE('',*,*,#1941,.F.) ;
#2555 = ORIENTED_EDGE('',*,*,#1940,.F.) ;
#2556 = ORIENTED_EDGE('',*,*,#1948,.T.) ;
#2557 = ORIENTED_EDGE('',*,*,#1944,.F.) ;
#2558 = ORIENTED_EDGE('',*,*,#1895,.F.) ;
#2559 = ORIENTED_EDGE('',*,*,#1950,.T.) ;
#2560 = ORIENTED_EDGE('',*,*,#1935,.F.) ;
#2561 = ORIENTED_EDGE('',*,*,#1949,.T.) ;
#2562 = ORIENTED_EDGE('',*,*,#1943,.F.) ;
#2563 = ORIENTED_EDGE('',*,*,#1951,.T.) ;
#2564 = ORIENTED_EDGE('',*,*,#1931,.F.) ;
#2565 = ORIENTED_EDGE('',*,*,#1936,.F.) ;
#2566 = ORIENTED_EDGE('',*,*,#1950,.F.) ;
#2567 = ORIENTED_EDGE('',*,*,#1894,.F.) ;
#2568 = ORIENTED_EDGE('',*,*,#1893,.F.) ;
#2569 = ORIENTED_EDGE('',*,*,#1951,.F.) ;
#2570 = ORIENTED_EDGE('',*,*,#1942,.F.) ;
#2571 = ORIENTED_EDGE('',*,*,#1932,.F.) ;
#2572 = ORIENTED_EDGE('',*,*,#1896,.F.) ;
#2573 = ORIENTED_EDGE('',*,*,#1875,.T.) ;
#2574 = ORIENTED_EDGE('',*,*,#1952,.F.) ;
#2575 = ORIENTED_EDGE('',*,*,#1953,.T.) ;
#2576 = ORIENTED_EDGE('',*,*,#1902,.T.) ;
#2577 = ORIENTED_EDGE('',*,*,#1954,.T.) ;
#2578 = ORIENTED_EDGE('',*,*,#1955,.F.) ;
#2579 = ORIENTED_EDGE('',*,*,#1956,.F.) ;
#2580 = ORIENTED_EDGE('',*,*,#1957,.T.) ;
#2581 = ORIENTED_EDGE('',*,*,#1958,.T.) ;
#2582 = ORIENTED_EDGE('',*,*,#1952,.T.) ;
#2583 = ORIENTED_EDGE('',*,*,#1959,.T.) ;
#2584 = ORIENTED_EDGE('',*,*,#1960,.T.) ;
#2585 = ORIENTED_EDGE('',*,*,#1961,.T.) ;
#2586 = ORIENTED_EDGE('',*,*,#1962,.T.) ;
#2587 = ORIENTED_EDGE('',*,*,#1963,.T.) ;
#2588 = ORIENTED_EDGE('',*,*,#1955,.T.) ;
#2589 = ORIENTED_EDGE('',*,*,#1964,.T.) ;
#2590 = ORIENTED_EDGE('',*,*,#1965,.T.) ;
#2591 = ORIENTED_EDGE('',*,*,#1966,.T.) ;
#2592 = ORIENTED_EDGE('',*,*,#1967,.F.) ;
#2593 = ORIENTED_EDGE('',*,*,#1968,.T.) ;
#2594 = ORIENTED_EDGE('',*,*,#1969,.F.) ;
#2595 = ORIENTED_EDGE('',*,*,#1960,.F.) ;
#2596 = ORIENTED_EDGE('',*,*,#1959,.F.) ;
#2597 = ORIENTED_EDGE('',*,*,#1956,.T.) ;
#2598 = ORIENTED_EDGE('',*,*,#1968,.F.) ;
#2599 = ORIENTED_EDGE('',*,*,#1969,.T.) ;
#2600 = ORIENTED_EDGE('',*,*,#1967,.T.) ;
#2601 = ORIENTED_EDGE('',*,*,#1970,.F.) ;
#2602 = ORIENTED_EDGE('',*,*,#1961,.F.) ;
#2603 = ORIENTED_EDGE('',*,*,#1971,.F.) ;
#2604 = ORIENTED_EDGE('',*,*,#1963,.F.) ;
#2605 = ORIENTED_EDGE('',*,*,#1962,.F.) ;
#2606 = ORIENTED_EDGE('',*,*,#1970,.T.) ;
#2607 = ORIENTED_EDGE('',*,*,#1966,.F.) ;
#2608 = ORIENTED_EDGE('',*,*,#1900,.F.) ;
#2609 = ORIENTED_EDGE('',*,*,#1972,.T.) ;
#2610 = ORIENTED_EDGE('',*,*,#1957,.F.) ;
#2611 = ORIENTED_EDGE('',*,*,#1971,.T.) ;
#2612 = ORIENTED_EDGE('',*,*,#1965,.F.) ;
#2613 = ORIENTED_EDGE('',*,*,#1973,.T.) ;
#2614 = ORIENTED_EDGE('',*,*,#1953,.F.) ;
#2615 = ORIENTED_EDGE('',*,*,#1958,.F.) ;
#2616 = ORIENTED_EDGE('',*,*,#1972,.F.) ;
#2617 = ORIENTED_EDGE('',*,*,#1899,.F.) ;
#2618 = ORIENTED_EDGE('',*,*,#1898,.F.) ;
#2619 = ORIENTED_EDGE('',*,*,#1973,.F.) ;
#2620 = ORIENTED_EDGE('',*,*,#1964,.F.) ;
#2621 = ORIENTED_EDGE('',*,*,#1954,.F.) ;
#2622 = ORIENTED_EDGE('',*,*,#1901,.F.) ;
#2623 = ORIENTED_EDGE('',*,*,#1974,.F.) ;
#2624 = ORIENTED_EDGE('',*,*,#1975,.T.) ;
#2625 = ORIENTED_EDGE('',*,*,#1891,.T.) ;
#2626 = ORIENTED_EDGE('',*,*,#1976,.T.) ;
#2627 = ORIENTED_EDGE('',*,*,#1977,.F.) ;
#2628 = ORIENTED_EDGE('',*,*,#1978,.F.) ;
#2629 = ORIENTED_EDGE('',*,*,#1979,.T.) ;
#2630 = ORIENTED_EDGE('',*,*,#1980,.T.) ;
#2631 = ORIENTED_EDGE('',*,*,#1974,.T.) ;
#2632 = ORIENTED_EDGE('',*,*,#1981,.T.) ;
#2633 = ORIENTED_EDGE('',*,*,#1982,.T.) ;
#2634 = ORIENTED_EDGE('',*,*,#1983,.T.) ;
#2635 = ORIENTED_EDGE('',*,*,#1984,.T.) ;
#2636 = ORIENTED_EDGE('',*,*,#1985,.T.) ;
#2637 = ORIENTED_EDGE('',*,*,#1977,.T.) ;
#2638 = ORIENTED_EDGE('',*,*,#1986,.T.) ;
#2639 = ORIENTED_EDGE('',*,*,#1987,.T.) ;
#2640 = ORIENTED_EDGE('',*,*,#1988,.T.) ;
#2641 = ORIENTED_EDGE('',*,*,#1989,.F.) ;
#2642 = ORIENTED_EDGE('',*,*,#1990,.T.) ;
#2643 = ORIENTED_EDGE('',*,*,#1991,.F.) ;
#2644 = ORIENTED_EDGE('',*,*,#1982,.F.) ;
#2645 = ORIENTED_EDGE('',*,*,#1981,.F.) ;
#2646 = ORIENTED_EDGE('',*,*,#1978,.T.) ;
#2647 = ORIENTED_EDGE('',*,*,#1990,.F.) ;
#2648 = ORIENTED_EDGE('',*,*,#1991,.T.) ;
#2649 = ORIENTED_EDGE('',*,*,#1989,.T.) ;
#2650 = ORIENTED_EDGE('',*,*,#1992,.F.) ;
#2651 = ORIENTED_EDGE('',*,*,#1983,.F.) ;
#2652 = ORIENTED_EDGE('',*,*,#1993,.F.) ;
#2653 = ORIENTED_EDGE('',*,*,#1985,.F.) ;
#2654 = ORIENTED_EDGE('',*,*,#1984,.F.) ;
#2655 = ORIENTED_EDGE('',*,*,#1992,.T.) ;
#2656 = ORIENTED_EDGE('',*,*,#1988,.F.) ;
#2657 = ORIENTED_EDGE('',*,*,#1888,.F.) ;
#2658 = ORIENTED_EDGE('',*,*,#1994,.T.) ;
#2659 = ORIENTED_EDGE('',*,*,#1979,.F.) ;
#2660 = ORIENTED_EDGE('',*,*,#1993,.T.) ;
#2661 = ORIENTED_EDGE('',*,*,#1987,.F.) ;
#2662 = ORIENTED_EDGE('',*,*,#1995,.T.) ;
#2663 = ORIENTED_EDGE('',*,*,#1975,.F.) ;
#2664 = ORIENTED_EDGE('',*,*,#1980,.F.) ;
#2665 = ORIENTED_EDGE('',*,*,#1994,.F.) ;
#2666 = ORIENTED_EDGE('',*,*,#1887,.F.) ;
#2667 = ORIENTED_EDGE('',*,*,#1886,.F.) ;
#2668 = ORIENTED_EDGE('',*,*,#1892,.F.) ;
#2669 = ORIENTED_EDGE('',*,*,#1995,.F.) ;
#2670 = ORIENTED_EDGE('',*,*,#1986,.F.) ;
#2671 = ORIENTED_EDGE('',*,*,#1976,.F.) ;
#2672 = ORIENTED_EDGE('',*,*,#1890,.F.) ;
#2673 = ORIENTED_EDGE('',*,*,#1889,.F.) ;
#2674 = ORIENTED_EDGE('',*,*,#1996,.F.) ;
#2675 = ORIENTED_EDGE('',*,*,#1997,.T.) ;
#2676 = ORIENTED_EDGE('',*,*,#1907,.T.) ;
#2677 = ORIENTED_EDGE('',*,*,#1998,.T.) ;
#2678 = ORIENTED_EDGE('',*,*,#1999,.F.) ;
#2679 = ORIENTED_EDGE('',*,*,#2000,.F.) ;
#2680 = ORIENTED_EDGE('',*,*,#2001,.T.) ;
#2681 = ORIENTED_EDGE('',*,*,#2002,.T.) ;
#2682 = ORIENTED_EDGE('',*,*,#1996,.T.) ;
#2683 = ORIENTED_EDGE('',*,*,#2003,.T.) ;
#2684 = ORIENTED_EDGE('',*,*,#2004,.T.) ;
#2685 = ORIENTED_EDGE('',*,*,#2005,.T.) ;
#2686 = ORIENTED_EDGE('',*,*,#2006,.T.) ;
#2687 = ORIENTED_EDGE('',*,*,#2007,.T.) ;
#2688 = ORIENTED_EDGE('',*,*,#1999,.T.) ;
#2689 = ORIENTED_EDGE('',*,*,#2008,.T.) ;
#2690 = ORIENTED_EDGE('',*,*,#2009,.T.) ;
#2691 = ORIENTED_EDGE('',*,*,#2010,.T.) ;
#2692 = ORIENTED_EDGE('',*,*,#2011,.F.) ;
#2693 = ORIENTED_EDGE('',*,*,#2012,.T.) ;
#2694 = ORIENTED_EDGE('',*,*,#2013,.F.) ;
#2695 = ORIENTED_EDGE('',*,*,#2004,.F.) ;
#2696 = ORIENTED_EDGE('',*,*,#2003,.F.) ;
#2697 = ORIENTED_EDGE('',*,*,#2000,.T.) ;
#2698 = ORIENTED_EDGE('',*,*,#2012,.F.) ;
#2699 = ORIENTED_EDGE('',*,*,#2013,.T.) ;
#2700 = ORIENTED_EDGE('',*,*,#2011,.T.) ;
#2701 = ORIENTED_EDGE('',*,*,#2014,.F.) ;
#2702 = ORIENTED_EDGE('',*,*,#2005,.F.) ;
#2703 = ORIENTED_EDGE('',*,*,#2015,.F.) ;
#2704 = ORIENTED_EDGE('',*,*,#2007,.F.) ;
#2705 = ORIENTED_EDGE('',*,*,#2006,.F.) ;
#2706 = ORIENTED_EDGE('',*,*,#2014,.T.) ;
#2707 = ORIENTED_EDGE('',*,*,#2010,.F.) ;
#2708 = ORIENTED_EDGE('',*,*,#1905,.F.) ;
#2709 = ORIENTED_EDGE('',*,*,#2016,.T.) ;
#2710 = ORIENTED_EDGE('',*,*,#2001,.F.) ;
#2711 = ORIENTED_EDGE('',*,*,#2015,.T.) ;
#2712 = ORIENTED_EDGE('',*,*,#2009,.F.) ;
#2713 = ORIENTED_EDGE('',*,*,#2017,.T.) ;
#2714 = ORIENTED_EDGE('',*,*,#1997,.F.) ;
#2715 = ORIENTED_EDGE('',*,*,#2002,.F.) ;
#2716 = ORIENTED_EDGE('',*,*,#2016,.F.) ;
#2717 = ORIENTED_EDGE('',*,*,#1904,.F.) ;
#2718 = ORIENTED_EDGE('',*,*,#1903,.F.) ;
#2719 = ORIENTED_EDGE('',*,*,#2017,.F.) ;
#2720 = ORIENTED_EDGE('',*,*,#2008,.F.) ;
#2721 = ORIENTED_EDGE('',*,*,#1998,.F.) ;
#2722 = ORIENTED_EDGE('',*,*,#1906,.F.) ;
#2723 = ORIENTED_EDGE('',*,*,#2018,.T.) ;
#2724 = ORIENTED_EDGE('',*,*,#2019,.T.) ;
#2725 = ORIENTED_EDGE('',*,*,#2020,.F.) ;
#2726 = ORIENTED_EDGE('',*,*,#2019,.F.) ;
#2727 = ORIENTED_EDGE('',*,*,#2021,.T.) ;
#2728 = ORIENTED_EDGE('',*,*,#2022,.T.) ;
#2729 = ORIENTED_EDGE('',*,*,#2023,.F.) ;
#2730 = ORIENTED_EDGE('',*,*,#2022,.F.) ;
#2731 = ORIENTED_EDGE('',*,*,#2023,.T.) ;
#2732 = ORIENTED_EDGE('',*,*,#2018,.F.) ;
#2733 = ORIENTED_EDGE('',*,*,#2021,.F.) ;
#2734 = ORIENTED_EDGE('',*,*,#2020,.T.) ;
#2735 = ORIENTED_EDGE('',*,*,#2024,.T.) ;
#2736 = ORIENTED_EDGE('',*,*,#2025,.T.) ;
#2737 = ORIENTED_EDGE('',*,*,#2026,.F.) ;
#2738 = ORIENTED_EDGE('',*,*,#2027,.T.) ;
#2739 = ORIENTED_EDGE('',*,*,#2028,.T.) ;
#2740 = ORIENTED_EDGE('',*,*,#2029,.T.) ;
#2741 = ORIENTED_EDGE('',*,*,#2030,.F.) ;
#2742 = ORIENTED_EDGE('',*,*,#2031,.T.) ;
#2743 = ORIENTED_EDGE('',*,*,#2032,.F.) ;
#2744 = ORIENTED_EDGE('',*,*,#2033,.T.) ;
#2745 = ORIENTED_EDGE('',*,*,#2034,.T.) ;
#2746 = ORIENTED_EDGE('',*,*,#2035,.T.) ;
#2747 = ORIENTED_EDGE('',*,*,#2036,.T.) ;
#2748 = ORIENTED_EDGE('',*,*,#2037,.T.) ;
#2749 = ORIENTED_EDGE('',*,*,#2038,.F.) ;
#2750 = ORIENTED_EDGE('',*,*,#2039,.T.) ;
#2751 = ORIENTED_EDGE('',*,*,#2030,.T.) ;
#2752 = ORIENTED_EDGE('',*,*,#2040,.T.) ;
#2753 = ORIENTED_EDGE('',*,*,#2032,.T.) ;
#2754 = ORIENTED_EDGE('',*,*,#2041,.T.) ;
#2755 = ORIENTED_EDGE('',*,*,#2038,.T.) ;
#2756 = ORIENTED_EDGE('',*,*,#2042,.T.) ;
#2757 = ORIENTED_EDGE('',*,*,#2026,.T.) ;
#2758 = ORIENTED_EDGE('',*,*,#2043,.T.) ;
#2759 = ORIENTED_EDGE('',*,*,#2034,.F.) ;
#2760 = ORIENTED_EDGE('',*,*,#2044,.T.) ;
#2761 = ORIENTED_EDGE('',*,*,#2028,.F.) ;
#2762 = ORIENTED_EDGE('',*,*,#2045,.T.) ;
#2763 = ORIENTED_EDGE('',*,*,#2024,.F.) ;
#2764 = ORIENTED_EDGE('',*,*,#2046,.T.) ;
#2765 = ORIENTED_EDGE('',*,*,#2036,.F.) ;
#2766 = ORIENTED_EDGE('',*,*,#2047,.T.) ;
#2767 = ORIENTED_EDGE('',*,*,#2040,.F.) ;
#2768 = ORIENTED_EDGE('',*,*,#2029,.F.) ;
#2769 = ORIENTED_EDGE('',*,*,#2044,.F.) ;
#2770 = ORIENTED_EDGE('',*,*,#2033,.F.) ;
#2771 = ORIENTED_EDGE('',*,*,#2043,.F.) ;
#2772 = ORIENTED_EDGE('',*,*,#2025,.F.) ;
#2773 = ORIENTED_EDGE('',*,*,#2045,.F.) ;
#2774 = ORIENTED_EDGE('',*,*,#2031,.F.) ;
#2775 = ORIENTED_EDGE('',*,*,#2042,.F.) ;
#2776 = ORIENTED_EDGE('',*,*,#2037,.F.) ;
#2777 = ORIENTED_EDGE('',*,*,#2046,.F.) ;
#2778 = ORIENTED_EDGE('',*,*,#2027,.F.) ;
#2779 = ORIENTED_EDGE('',*,*,#2041,.F.) ;
#2780 = ORIENTED_EDGE('',*,*,#2035,.F.) ;
#2781 = ORIENTED_EDGE('',*,*,#2047,.F.) ;
#2782 = ORIENTED_EDGE('',*,*,#2039,.F.) ;
#2783 = ORIENTED_EDGE('',*,*,#2048,.F.) ;
#2784 = ORIENTED_EDGE('',*,*,#2049,.T.) ;
#2785 = ORIENTED_EDGE('',*,*,#2050,.T.) ;
#2786 = ORIENTED_EDGE('',*,*,#2049,.F.) ;
#2787 = ORIENTED_EDGE('',*,*,#2051,.F.) ;
#2788 = ORIENTED_EDGE('',*,*,#2052,.T.) ;
#2789 = ORIENTED_EDGE('',*,*,#2053,.F.) ;
#2790 = ORIENTED_EDGE('',*,*,#2054,.T.) ;
#2791 = ORIENTED_EDGE('',*,*,#2055,.F.) ;
#2792 = ORIENTED_EDGE('',*,*,#2056,.T.) ;
#2793 = ORIENTED_EDGE('',*,*,#2057,.F.) ;
#2794 = ORIENTED_EDGE('',*,*,#2058,.T.) ;
#2795 = ORIENTED_EDGE('',*,*,#2048,.T.) ;
#2796 = ORIENTED_EDGE('',*,*,#2059,.T.) ;
#2797 = ORIENTED_EDGE('',*,*,#2060,.T.) ;
#2798 = ORIENTED_EDGE('',*,*,#2061,.T.) ;
#2799 = ORIENTED_EDGE('',*,*,#2062,.T.) ;
#2800 = ORIENTED_EDGE('',*,*,#2063,.T.) ;
#2801 = ORIENTED_EDGE('',*,*,#2064,.T.) ;
#2802 = ORIENTED_EDGE('',*,*,#2065,.T.) ;
#2803 = ORIENTED_EDGE('',*,*,#2066,.T.) ;
#2804 = ORIENTED_EDGE('',*,*,#2050,.F.) ;
#2805 = ORIENTED_EDGE('',*,*,#2052,.F.) ;
#2806 = ORIENTED_EDGE('',*,*,#2067,.F.) ;
#2807 = ORIENTED_EDGE('',*,*,#2060,.F.) ;
#2808 = ORIENTED_EDGE('',*,*,#2068,.F.) ;
#2809 = ORIENTED_EDGE('',*,*,#2054,.F.) ;
#2810 = ORIENTED_EDGE('',*,*,#2069,.F.) ;
#2811 = ORIENTED_EDGE('',*,*,#2066,.F.) ;
#2812 = ORIENTED_EDGE('',*,*,#2070,.F.) ;
#2813 = ORIENTED_EDGE('',*,*,#2056,.F.) ;
#2814 = ORIENTED_EDGE('',*,*,#2071,.F.) ;
#2815 = ORIENTED_EDGE('',*,*,#2064,.F.) ;
#2816 = ORIENTED_EDGE('',*,*,#2072,.F.) ;
#2817 = ORIENTED_EDGE('',*,*,#2058,.F.) ;
#2818 = ORIENTED_EDGE('',*,*,#2073,.F.) ;
#2819 = ORIENTED_EDGE('',*,*,#2062,.F.) ;
#2820 = ORIENTED_EDGE('',*,*,#2074,.F.) ;
#2821 = ORIENTED_EDGE('',*,*,#2075,.F.) ;
#2822 = ORIENTED_EDGE('',*,*,#2076,.F.) ;
#2823 = ORIENTED_EDGE('',*,*,#2072,.T.) ;
#2824 = ORIENTED_EDGE('',*,*,#2077,.T.) ;
#2825 = ORIENTED_EDGE('',*,*,#2078,.F.) ;
#2826 = ORIENTED_EDGE('',*,*,#2079,.T.) ;
#2827 = ORIENTED_EDGE('',*,*,#2080,.T.) ;
#2828 = ORIENTED_EDGE('',*,*,#2073,.T.) ;
#2829 = ORIENTED_EDGE('',*,*,#2063,.F.) ;
#2830 = ORIENTED_EDGE('',*,*,#2080,.F.) ;
#2831 = ORIENTED_EDGE('',*,*,#2081,.T.) ;
#2832 = ORIENTED_EDGE('',*,*,#2077,.F.) ;
#2833 = ORIENTED_EDGE('',*,*,#2057,.T.) ;
#2834 = ORIENTED_EDGE('',*,*,#2076,.T.) ;
#2835 = ORIENTED_EDGE('',*,*,#2082,.T.) ;
#2836 = ORIENTED_EDGE('',*,*,#2078,.T.) ;
#2837 = ORIENTED_EDGE('',*,*,#2079,.F.) ;
#2838 = ORIENTED_EDGE('',*,*,#2083,.T.) ;
#2839 = ORIENTED_EDGE('',*,*,#2084,.F.) ;
#2840 = ORIENTED_EDGE('',*,*,#2085,.F.) ;
#2841 = ORIENTED_EDGE('',*,*,#2075,.T.) ;
#2842 = ORIENTED_EDGE('',*,*,#2086,.F.) ;
#2843 = ORIENTED_EDGE('',*,*,#2087,.T.) ;
#2844 = ORIENTED_EDGE('',*,*,#2088,.T.) ;
#2845 = ORIENTED_EDGE('',*,*,#2081,.F.) ;
#2846 = ORIENTED_EDGE('',*,*,#2085,.T.) ;
#2847 = ORIENTED_EDGE('',*,*,#2089,.T.) ;
#2848 = ORIENTED_EDGE('',*,*,#2086,.T.) ;
#2849 = ORIENTED_EDGE('',*,*,#2083,.F.) ;
#2850 = ORIENTED_EDGE('',*,*,#2082,.F.) ;
#2851 = ORIENTED_EDGE('',*,*,#2088,.F.) ;
#2852 = ORIENTED_EDGE('',*,*,#2090,.F.) ;
#2853 = ORIENTED_EDGE('',*,*,#2090,.T.) ;
#2854 = ORIENTED_EDGE('',*,*,#2087,.F.) ;
#2855 = ORIENTED_EDGE('',*,*,#2089,.F.) ;
#2856 = ORIENTED_EDGE('',*,*,#2084,.T.) ;
#2857 = ORIENTED_EDGE('',*,*,#2091,.F.) ;
#2858 = ORIENTED_EDGE('',*,*,#2092,.F.) ;
#2859 = ORIENTED_EDGE('',*,*,#2074,.T.) ;
#2860 = ORIENTED_EDGE('',*,*,#2093,.T.) ;
#2861 = ORIENTED_EDGE('',*,*,#2094,.F.) ;
#2862 = ORIENTED_EDGE('',*,*,#2095,.T.) ;
#2863 = ORIENTED_EDGE('',*,*,#2096,.T.) ;
#2864 = ORIENTED_EDGE('',*,*,#2067,.T.) ;
#2865 = ORIENTED_EDGE('',*,*,#2061,.F.) ;
#2866 = ORIENTED_EDGE('',*,*,#2096,.F.) ;
#2867 = ORIENTED_EDGE('',*,*,#2097,.T.) ;
#2868 = ORIENTED_EDGE('',*,*,#2093,.F.) ;
#2869 = ORIENTED_EDGE('',*,*,#2051,.T.) ;
#2870 = ORIENTED_EDGE('',*,*,#2092,.T.) ;
#2871 = ORIENTED_EDGE('',*,*,#2098,.T.) ;
#2872 = ORIENTED_EDGE('',*,*,#2094,.T.) ;
#2873 = ORIENTED_EDGE('',*,*,#2095,.F.) ;
#2874 = ORIENTED_EDGE('',*,*,#2099,.T.) ;
#2875 = ORIENTED_EDGE('',*,*,#2100,.F.) ;
#2876 = ORIENTED_EDGE('',*,*,#2101,.F.) ;
#2877 = ORIENTED_EDGE('',*,*,#2091,.T.) ;
#2878 = ORIENTED_EDGE('',*,*,#2102,.F.) ;
#2879 = ORIENTED_EDGE('',*,*,#2103,.T.) ;
#2880 = ORIENTED_EDGE('',*,*,#2104,.T.) ;
#2881 = ORIENTED_EDGE('',*,*,#2097,.F.) ;
#2882 = ORIENTED_EDGE('',*,*,#2101,.T.) ;
#2883 = ORIENTED_EDGE('',*,*,#2105,.T.) ;
#2884 = ORIENTED_EDGE('',*,*,#2102,.T.) ;
#2885 = ORIENTED_EDGE('',*,*,#2099,.F.) ;
#2886 = ORIENTED_EDGE('',*,*,#2098,.F.) ;
#2887 = ORIENTED_EDGE('',*,*,#2104,.F.) ;
#2888 = ORIENTED_EDGE('',*,*,#2106,.F.) ;
#2889 = ORIENTED_EDGE('',*,*,#2106,.T.) ;
#2890 = ORIENTED_EDGE('',*,*,#2103,.F.) ;
#2891 = ORIENTED_EDGE('',*,*,#2105,.F.) ;
#2892 = ORIENTED_EDGE('',*,*,#2100,.T.) ;
#2893 = ORIENTED_EDGE('',*,*,#2107,.F.) ;
#2894 = ORIENTED_EDGE('',*,*,#2108,.F.) ;
#2895 = ORIENTED_EDGE('',*,*,#2068,.T.) ;
#2896 = ORIENTED_EDGE('',*,*,#2109,.T.) ;
#2897 = ORIENTED_EDGE('',*,*,#2110,.F.) ;
#2898 = ORIENTED_EDGE('',*,*,#2111,.T.) ;
#2899 = ORIENTED_EDGE('',*,*,#2112,.T.) ;
#2900 = ORIENTED_EDGE('',*,*,#2069,.T.) ;
#2901 = ORIENTED_EDGE('',*,*,#2059,.F.) ;
#2902 = ORIENTED_EDGE('',*,*,#2112,.F.) ;
#2903 = ORIENTED_EDGE('',*,*,#2113,.T.) ;
#2904 = ORIENTED_EDGE('',*,*,#2109,.F.) ;
#2905 = ORIENTED_EDGE('',*,*,#2053,.T.) ;
#2906 = ORIENTED_EDGE('',*,*,#2108,.T.) ;
#2907 = ORIENTED_EDGE('',*,*,#2114,.T.) ;
#2908 = ORIENTED_EDGE('',*,*,#2110,.T.) ;
#2909 = ORIENTED_EDGE('',*,*,#2111,.F.) ;
#2910 = ORIENTED_EDGE('',*,*,#2115,.T.) ;
#2911 = ORIENTED_EDGE('',*,*,#2116,.F.) ;
#2912 = ORIENTED_EDGE('',*,*,#2117,.F.) ;
#2913 = ORIENTED_EDGE('',*,*,#2107,.T.) ;
#2914 = ORIENTED_EDGE('',*,*,#2118,.F.) ;
#2915 = ORIENTED_EDGE('',*,*,#2119,.T.) ;
#2916 = ORIENTED_EDGE('',*,*,#2120,.T.) ;
#2917 = ORIENTED_EDGE('',*,*,#2113,.F.) ;
#2918 = ORIENTED_EDGE('',*,*,#2117,.T.) ;
#2919 = ORIENTED_EDGE('',*,*,#2121,.T.) ;
#2920 = ORIENTED_EDGE('',*,*,#2118,.T.) ;
#2921 = ORIENTED_EDGE('',*,*,#2115,.F.) ;
#2922 = ORIENTED_EDGE('',*,*,#2114,.F.) ;
#2923 = ORIENTED_EDGE('',*,*,#2120,.F.) ;
#2924 = ORIENTED_EDGE('',*,*,#2122,.F.) ;
#2925 = ORIENTED_EDGE('',*,*,#2122,.T.) ;
#2926 = ORIENTED_EDGE('',*,*,#2119,.F.) ;
#2927 = ORIENTED_EDGE('',*,*,#2121,.F.) ;
#2928 = ORIENTED_EDGE('',*,*,#2116,.T.) ;
#2929 = ORIENTED_EDGE('',*,*,#2123,.F.) ;
#2930 = ORIENTED_EDGE('',*,*,#2124,.F.) ;
#2931 = ORIENTED_EDGE('',*,*,#2070,.T.) ;
#2932 = ORIENTED_EDGE('',*,*,#2125,.T.) ;
#2933 = ORIENTED_EDGE('',*,*,#2126,.F.) ;
#2934 = ORIENTED_EDGE('',*,*,#2127,.T.) ;
#2935 = ORIENTED_EDGE('',*,*,#2128,.T.) ;
#2936 = ORIENTED_EDGE('',*,*,#2071,.T.) ;
#2937 = ORIENTED_EDGE('',*,*,#2065,.F.) ;
#2938 = ORIENTED_EDGE('',*,*,#2128,.F.) ;
#2939 = ORIENTED_EDGE('',*,*,#2129,.T.) ;
#2940 = ORIENTED_EDGE('',*,*,#2125,.F.) ;
#2941 = ORIENTED_EDGE('',*,*,#2055,.T.) ;
#2942 = ORIENTED_EDGE('',*,*,#2124,.T.) ;
#2943 = ORIENTED_EDGE('',*,*,#2130,.T.) ;
#2944 = ORIENTED_EDGE('',*,*,#2126,.T.) ;
#2945 = ORIENTED_EDGE('',*,*,#2127,.F.) ;
#2946 = ORIENTED_EDGE('',*,*,#2131,.T.) ;
#2947 = ORIENTED_EDGE('',*,*,#2132,.F.) ;
#2948 = ORIENTED_EDGE('',*,*,#2133,.F.) ;
#2949 = ORIENTED_EDGE('',*,*,#2123,.T.) ;
#2950 = ORIENTED_EDGE('',*,*,#2134,.F.) ;
#2951 = ORIENTED_EDGE('',*,*,#2135,.T.) ;
#2952 = ORIENTED_EDGE('',*,*,#2136,.T.) ;
#2953 = ORIENTED_EDGE('',*,*,#2129,.F.) ;
#2954 = ORIENTED_EDGE('',*,*,#2133,.T.) ;
#2955 = ORIENTED_EDGE('',*,*,#2137,.T.) ;
#2956 = ORIENTED_EDGE('',*,*,#2134,.T.) ;
#2957 = ORIENTED_EDGE('',*,*,#2131,.F.) ;
#2958 = ORIENTED_EDGE('',*,*,#2130,.F.) ;
#2959 = ORIENTED_EDGE('',*,*,#2136,.F.) ;
#2960 = ORIENTED_EDGE('',*,*,#2138,.F.) ;
#2961 = ORIENTED_EDGE('',*,*,#2138,.T.) ;
#2962 = ORIENTED_EDGE('',*,*,#2135,.F.) ;
#2963 = ORIENTED_EDGE('',*,*,#2137,.F.) ;
#2964 = ORIENTED_EDGE('',*,*,#2132,.T.) ;
#2965 = ORIENTED_EDGE('',*,*,#2139,.F.) ;
#2966 = ORIENTED_EDGE('',*,*,#2140,.T.) ;
#2967 = ORIENTED_EDGE('',*,*,#2141,.T.) ;
#2968 = ORIENTED_EDGE('',*,*,#2142,.T.) ;
#2969 = ORIENTED_EDGE('',*,*,#2140,.F.) ;
#2970 = ORIENTED_EDGE('',*,*,#2143,.F.) ;
#2971 = ORIENTED_EDGE('',*,*,#2144,.T.) ;
#2972 = ORIENTED_EDGE('',*,*,#2145,.T.) ;
#2973 = ORIENTED_EDGE('',*,*,#2144,.F.) ;
#2974 = ORIENTED_EDGE('',*,*,#2146,.F.) ;
#2975 = ORIENTED_EDGE('',*,*,#2147,.F.) ;
#2976 = ORIENTED_EDGE('',*,*,#2148,.T.) ;
#2977 = ORIENTED_EDGE('',*,*,#2149,.T.) ;
#2978 = ORIENTED_EDGE('',*,*,#2150,.T.) ;
#2979 = ORIENTED_EDGE('',*,*,#2148,.F.) ;
#2980 = ORIENTED_EDGE('',*,*,#2151,.T.) ;
#2981 = ORIENTED_EDGE('',*,*,#2152,.T.) ;
#2982 = ORIENTED_EDGE('',*,*,#2153,.F.) ;
#2983 = ORIENTED_EDGE('',*,*,#2154,.F.) ;
#2984 = ORIENTED_EDGE('',*,*,#2152,.F.) ;
#2985 = ORIENTED_EDGE('',*,*,#2155,.T.) ;
#2986 = ORIENTED_EDGE('',*,*,#2156,.F.) ;
#2987 = ORIENTED_EDGE('',*,*,#2157,.F.) ;
#2988 = ORIENTED_EDGE('',*,*,#2158,.T.) ;
#2989 = ORIENTED_EDGE('',*,*,#2159,.T.) ;
#2990 = ORIENTED_EDGE('',*,*,#2160,.T.) ;
#2991 = ORIENTED_EDGE('',*,*,#2158,.F.) ;
#2992 = ORIENTED_EDGE('',*,*,#2161,.F.) ;
#2993 = ORIENTED_EDGE('',*,*,#2162,.F.) ;
#2994 = ORIENTED_EDGE('',*,*,#2163,.T.) ;
#2995 = ORIENTED_EDGE('',*,*,#2164,.T.) ;
#2996 = ORIENTED_EDGE('',*,*,#2163,.F.) ;
#2997 = ORIENTED_EDGE('',*,*,#2165,.F.) ;
#2998 = ORIENTED_EDGE('',*,*,#2166,.T.) ;
#2999 = ORIENTED_EDGE('',*,*,#2167,.T.) ;
#3000 = ORIENTED_EDGE('',*,*,#2166,.F.) ;
#3001 = ORIENTED_EDGE('',*,*,#2168,.F.) ;
#3002 = ORIENTED_EDGE('',*,*,#2169,.F.) ;
#3003 = ORIENTED_EDGE('',*,*,#2170,.T.) ;
#3004 = ORIENTED_EDGE('',*,*,#2171,.T.) ;
#3005 = ORIENTED_EDGE('',*,*,#2172,.T.) ;
#3006 = ORIENTED_EDGE('',*,*,#2170,.F.) ;
#3007 = ORIENTED_EDGE('',*,*,#2156,.T.) ;
#3008 = ORIENTED_EDGE('',*,*,#2157,.T.) ;
#3009 = ORIENTED_EDGE('',*,*,#2173,.T.) ;
#3010 = ORIENTED_EDGE('',*,*,#2141,.F.) ;
#3011 = ORIENTED_EDGE('',*,*,#2142,.F.) ;
#3012 = ORIENTED_EDGE('',*,*,#2173,.F.) ;
#3013 = ORIENTED_EDGE('',*,*,#2139,.T.) ;
#3014 = ORIENTED_EDGE('',*,*,#2174,.T.) ;
#3015 = ORIENTED_EDGE('',*,*,#2145,.F.) ;
#3016 = ORIENTED_EDGE('',*,*,#2174,.F.) ;
#3017 = ORIENTED_EDGE('',*,*,#2143,.T.) ;
#3018 = ORIENTED_EDGE('',*,*,#2175,.T.) ;
#3019 = ORIENTED_EDGE('',*,*,#2149,.F.) ;
#3020 = ORIENTED_EDGE('',*,*,#2150,.F.) ;
#3021 = ORIENTED_EDGE('',*,*,#2175,.F.) ;
#3022 = ORIENTED_EDGE('',*,*,#2146,.T.) ;
#3023 = ORIENTED_EDGE('',*,*,#2147,.T.) ;
#3024 = ORIENTED_EDGE('',*,*,#2176,.T.) ;
#3025 = ORIENTED_EDGE('',*,*,#2155,.F.) ;
#3026 = ORIENTED_EDGE('',*,*,#2151,.F.) ;
#3027 = ORIENTED_EDGE('',*,*,#2176,.F.) ;
#3028 = ORIENTED_EDGE('',*,*,#2160,.F.) ;
#3029 = ORIENTED_EDGE('',*,*,#2177,.T.) ;
#3030 = ORIENTED_EDGE('',*,*,#2161,.T.) ;
#3031 = ORIENTED_EDGE('',*,*,#2162,.T.) ;
#3032 = ORIENTED_EDGE('',*,*,#2177,.F.) ;
#3033 = ORIENTED_EDGE('',*,*,#2159,.F.) ;
#3034 = ORIENTED_EDGE('',*,*,#2164,.F.) ;
#3035 = ORIENTED_EDGE('',*,*,#2178,.T.) ;
#3036 = ORIENTED_EDGE('',*,*,#2165,.T.) ;
#3037 = ORIENTED_EDGE('',*,*,#2178,.F.) ;
#3038 = ORIENTED_EDGE('',*,*,#2167,.F.) ;
#3039 = ORIENTED_EDGE('',*,*,#2179,.T.) ;
#3040 = ORIENTED_EDGE('',*,*,#2168,.T.) ;
#3041 = ORIENTED_EDGE('',*,*,#2169,.T.) ;
#3042 = ORIENTED_EDGE('',*,*,#2179,.F.) ;
#3043 = ORIENTED_EDGE('',*,*,#2172,.F.) ;
#3044 = ORIENTED_EDGE('',*,*,#2180,.T.) ;
#3045 = ORIENTED_EDGE('',*,*,#2153,.T.) ;
#3046 = ORIENTED_EDGE('',*,*,#2154,.T.) ;
#3047 = ORIENTED_EDGE('',*,*,#2180,.F.) ;
#3048 = ORIENTED_EDGE('',*,*,#2171,.F.) ;
#3049 = ORIENTED_EDGE('',*,*,#2181,.F.) ;
#3050 = ORIENTED_EDGE('',*,*,#2182,.T.) ;
#3051 = ORIENTED_EDGE('',*,*,#2183,.T.) ;
#3052 = ORIENTED_EDGE('',*,*,#2184,.T.) ;
#3053 = ORIENTED_EDGE('',*,*,#2182,.F.) ;
#3054 = ORIENTED_EDGE('',*,*,#2185,.F.) ;
#3055 = ORIENTED_EDGE('',*,*,#2186,.T.) ;
#3056 = ORIENTED_EDGE('',*,*,#2187,.T.) ;
#3057 = ORIENTED_EDGE('',*,*,#2186,.F.) ;
#3058 = ORIENTED_EDGE('',*,*,#2188,.F.) ;
#3059 = ORIENTED_EDGE('',*,*,#2189,.F.) ;
#3060 = ORIENTED_EDGE('',*,*,#2190,.T.) ;
#3061 = ORIENTED_EDGE('',*,*,#2191,.T.) ;
#3062 = ORIENTED_EDGE('',*,*,#2192,.T.) ;
#3063 = ORIENTED_EDGE('',*,*,#2190,.F.) ;
#3064 = ORIENTED_EDGE('',*,*,#2193,.T.) ;
#3065 = ORIENTED_EDGE('',*,*,#2194,.T.) ;
#3066 = ORIENTED_EDGE('',*,*,#2195,.F.) ;
#3067 = ORIENTED_EDGE('',*,*,#2196,.F.) ;
#3068 = ORIENTED_EDGE('',*,*,#2194,.F.) ;
#3069 = ORIENTED_EDGE('',*,*,#2197,.T.) ;
#3070 = ORIENTED_EDGE('',*,*,#2198,.F.) ;
#3071 = ORIENTED_EDGE('',*,*,#2199,.F.) ;
#3072 = ORIENTED_EDGE('',*,*,#2200,.T.) ;
#3073 = ORIENTED_EDGE('',*,*,#2201,.T.) ;
#3074 = ORIENTED_EDGE('',*,*,#2202,.T.) ;
#3075 = ORIENTED_EDGE('',*,*,#2200,.F.) ;
#3076 = ORIENTED_EDGE('',*,*,#2203,.F.) ;
#3077 = ORIENTED_EDGE('',*,*,#2204,.F.) ;
#3078 = ORIENTED_EDGE('',*,*,#2205,.T.) ;
#3079 = ORIENTED_EDGE('',*,*,#2206,.T.) ;
#3080 = ORIENTED_EDGE('',*,*,#2205,.F.) ;
#3081 = ORIENTED_EDGE('',*,*,#2207,.F.) ;
#3082 = ORIENTED_EDGE('',*,*,#2208,.T.) ;
#3083 = ORIENTED_EDGE('',*,*,#2209,.T.) ;
#3084 = ORIENTED_EDGE('',*,*,#2208,.F.) ;
#3085 = ORIENTED_EDGE('',*,*,#2210,.F.) ;
#3086 = ORIENTED_EDGE('',*,*,#2211,.F.) ;
#3087 = ORIENTED_EDGE('',*,*,#2212,.T.) ;
#3088 = ORIENTED_EDGE('',*,*,#2213,.T.) ;
#3089 = ORIENTED_EDGE('',*,*,#2214,.T.) ;
#3090 = ORIENTED_EDGE('',*,*,#2212,.F.) ;
#3091 = ORIENTED_EDGE('',*,*,#2198,.T.) ;
#3092 = ORIENTED_EDGE('',*,*,#2199,.T.) ;
#3093 = ORIENTED_EDGE('',*,*,#2215,.T.) ;
#3094 = ORIENTED_EDGE('',*,*,#2183,.F.) ;
#3095 = ORIENTED_EDGE('',*,*,#2184,.F.) ;
#3096 = ORIENTED_EDGE('',*,*,#2215,.F.) ;
#3097 = ORIENTED_EDGE('',*,*,#2181,.T.) ;
#3098 = ORIENTED_EDGE('',*,*,#2216,.T.) ;
#3099 = ORIENTED_EDGE('',*,*,#2187,.F.) ;
#3100 = ORIENTED_EDGE('',*,*,#2216,.F.) ;
#3101 = ORIENTED_EDGE('',*,*,#2185,.T.) ;
#3102 = ORIENTED_EDGE('',*,*,#2217,.T.) ;
#3103 = ORIENTED_EDGE('',*,*,#2191,.F.) ;
#3104 = ORIENTED_EDGE('',*,*,#2192,.F.) ;
#3105 = ORIENTED_EDGE('',*,*,#2217,.F.) ;
#3106 = ORIENTED_EDGE('',*,*,#2188,.T.) ;
#3107 = ORIENTED_EDGE('',*,*,#2189,.T.) ;
#3108 = ORIENTED_EDGE('',*,*,#2218,.T.) ;
#3109 = ORIENTED_EDGE('',*,*,#2197,.F.) ;
#3110 = ORIENTED_EDGE('',*,*,#2193,.F.) ;
#3111 = ORIENTED_EDGE('',*,*,#2218,.F.) ;
#3112 = ORIENTED_EDGE('',*,*,#2202,.F.) ;
#3113 = ORIENTED_EDGE('',*,*,#2219,.T.) ;
#3114 = ORIENTED_EDGE('',*,*,#2203,.T.) ;
#3115 = ORIENTED_EDGE('',*,*,#2204,.T.) ;
#3116 = ORIENTED_EDGE('',*,*,#2219,.F.) ;
#3117 = ORIENTED_EDGE('',*,*,#2201,.F.) ;
#3118 = ORIENTED_EDGE('',*,*,#2206,.F.) ;
#3119 = ORIENTED_EDGE('',*,*,#2220,.T.) ;
#3120 = ORIENTED_EDGE('',*,*,#2207,.T.) ;
#3121 = ORIENTED_EDGE('',*,*,#2220,.F.) ;
#3122 = ORIENTED_EDGE('',*,*,#2209,.F.) ;
#3123 = ORIENTED_EDGE('',*,*,#2221,.T.) ;
#3124 = ORIENTED_EDGE('',*,*,#2210,.T.) ;
#3125 = ORIENTED_EDGE('',*,*,#2211,.T.) ;
#3126 = ORIENTED_EDGE('',*,*,#2221,.F.) ;
#3127 = ORIENTED_EDGE('',*,*,#2214,.F.) ;
#3128 = ORIENTED_EDGE('',*,*,#2222,.T.) ;
#3129 = ORIENTED_EDGE('',*,*,#2195,.T.) ;
#3130 = ORIENTED_EDGE('',*,*,#2196,.T.) ;
#3131 = ORIENTED_EDGE('',*,*,#2222,.F.) ;
#3132 = ORIENTED_EDGE('',*,*,#2213,.F.) ;
#3133 = ORIENTED_EDGE('',*,*,#2223,.F.) ;
#3134 = ORIENTED_EDGE('',*,*,#2224,.T.) ;
#3135 = ORIENTED_EDGE('',*,*,#2225,.T.) ;
#3136 = ORIENTED_EDGE('',*,*,#2226,.T.) ;
#3137 = ORIENTED_EDGE('',*,*,#2224,.F.) ;
#3138 = ORIENTED_EDGE('',*,*,#2227,.F.) ;
#3139 = ORIENTED_EDGE('',*,*,#2228,.T.) ;
#3140 = ORIENTED_EDGE('',*,*,#2229,.T.) ;
#3141 = ORIENTED_EDGE('',*,*,#2228,.F.) ;
#3142 = ORIENTED_EDGE('',*,*,#2230,.F.) ;
#3143 = ORIENTED_EDGE('',*,*,#2231,.F.) ;
#3144 = ORIENTED_EDGE('',*,*,#2232,.T.) ;
#3145 = ORIENTED_EDGE('',*,*,#2233,.T.) ;
#3146 = ORIENTED_EDGE('',*,*,#2234,.T.) ;
#3147 = ORIENTED_EDGE('',*,*,#2232,.F.) ;
#3148 = ORIENTED_EDGE('',*,*,#2235,.T.) ;
#3149 = ORIENTED_EDGE('',*,*,#2236,.T.) ;
#3150 = ORIENTED_EDGE('',*,*,#2237,.F.) ;
#3151 = ORIENTED_EDGE('',*,*,#2238,.F.) ;
#3152 = ORIENTED_EDGE('',*,*,#2236,.F.) ;
#3153 = ORIENTED_EDGE('',*,*,#2239,.T.) ;
#3154 = ORIENTED_EDGE('',*,*,#2240,.F.) ;
#3155 = ORIENTED_EDGE('',*,*,#2241,.F.) ;
#3156 = ORIENTED_EDGE('',*,*,#2242,.T.) ;
#3157 = ORIENTED_EDGE('',*,*,#2243,.T.) ;
#3158 = ORIENTED_EDGE('',*,*,#2244,.T.) ;
#3159 = ORIENTED_EDGE('',*,*,#2242,.F.) ;
#3160 = ORIENTED_EDGE('',*,*,#2245,.F.) ;
#3161 = ORIENTED_EDGE('',*,*,#2246,.F.) ;
#3162 = ORIENTED_EDGE('',*,*,#2247,.T.) ;
#3163 = ORIENTED_EDGE('',*,*,#2248,.T.) ;
#3164 = ORIENTED_EDGE('',*,*,#2247,.F.) ;
#3165 = ORIENTED_EDGE('',*,*,#2249,.F.) ;
#3166 = ORIENTED_EDGE('',*,*,#2250,.T.) ;
#3167 = ORIENTED_EDGE('',*,*,#2251,.T.) ;
#3168 = ORIENTED_EDGE('',*,*,#2250,.F.) ;
#3169 = ORIENTED_EDGE('',*,*,#2252,.F.) ;
#3170 = ORIENTED_EDGE('',*,*,#2253,.F.) ;
#3171 = ORIENTED_EDGE('',*,*,#2254,.T.) ;
#3172 = ORIENTED_EDGE('',*,*,#2255,.T.) ;
#3173 = ORIENTED_EDGE('',*,*,#2256,.T.) ;
#3174 = ORIENTED_EDGE('',*,*,#2254,.F.) ;
#3175 = ORIENTED_EDGE('',*,*,#2240,.T.) ;
#3176 = ORIENTED_EDGE('',*,*,#2241,.T.) ;
#3177 = ORIENTED_EDGE('',*,*,#2257,.T.) ;
#3178 = ORIENTED_EDGE('',*,*,#2225,.F.) ;
#3179 = ORIENTED_EDGE('',*,*,#2226,.F.) ;
#3180 = ORIENTED_EDGE('',*,*,#2257,.F.) ;
#3181 = ORIENTED_EDGE('',*,*,#2223,.T.) ;
#3182 = ORIENTED_EDGE('',*,*,#2258,.T.) ;
#3183 = ORIENTED_EDGE('',*,*,#2229,.F.) ;
#3184 = ORIENTED_EDGE('',*,*,#2258,.F.) ;
#3185 = ORIENTED_EDGE('',*,*,#2227,.T.) ;
#3186 = ORIENTED_EDGE('',*,*,#2259,.T.) ;
#3187 = ORIENTED_EDGE('',*,*,#2233,.F.) ;
#3188 = ORIENTED_EDGE('',*,*,#2234,.F.) ;
#3189 = ORIENTED_EDGE('',*,*,#2259,.F.) ;
#3190 = ORIENTED_EDGE('',*,*,#2230,.T.) ;
#3191 = ORIENTED_EDGE('',*,*,#2231,.T.) ;
#3192 = ORIENTED_EDGE('',*,*,#2260,.T.) ;
#3193 = ORIENTED_EDGE('',*,*,#2239,.F.) ;
#3194 = ORIENTED_EDGE('',*,*,#2235,.F.) ;
#3195 = ORIENTED_EDGE('',*,*,#2260,.F.) ;
#3196 = ORIENTED_EDGE('',*,*,#2244,.F.) ;
#3197 = ORIENTED_EDGE('',*,*,#2261,.T.) ;
#3198 = ORIENTED_EDGE('',*,*,#2245,.T.) ;
#3199 = ORIENTED_EDGE('',*,*,#2246,.T.) ;
#3200 = ORIENTED_EDGE('',*,*,#2261,.F.) ;
#3201 = ORIENTED_EDGE('',*,*,#2243,.F.) ;
#3202 = ORIENTED_EDGE('',*,*,#2248,.F.) ;
#3203 = ORIENTED_EDGE('',*,*,#2262,.T.) ;
#3204 = ORIENTED_EDGE('',*,*,#2249,.T.) ;
#3205 = ORIENTED_EDGE('',*,*,#2262,.F.) ;
#3206 = ORIENTED_EDGE('',*,*,#2251,.F.) ;
#3207 = ORIENTED_EDGE('',*,*,#2263,.T.) ;
#3208 = ORIENTED_EDGE('',*,*,#2252,.T.) ;
#3209 = ORIENTED_EDGE('',*,*,#2253,.T.) ;
#3210 = ORIENTED_EDGE('',*,*,#2263,.F.) ;
#3211 = ORIENTED_EDGE('',*,*,#2256,.F.) ;
#3212 = ORIENTED_EDGE('',*,*,#2264,.T.) ;
#3213 = ORIENTED_EDGE('',*,*,#2237,.T.) ;
#3214 = ORIENTED_EDGE('',*,*,#2238,.T.) ;
#3215 = ORIENTED_EDGE('',*,*,#2264,.F.) ;
#3216 = ORIENTED_EDGE('',*,*,#2255,.F.) ;
#3217 = ORIENTED_EDGE('',*,*,#2265,.F.) ;
#3218 = ORIENTED_EDGE('',*,*,#2266,.T.) ;
#3219 = ORIENTED_EDGE('',*,*,#2267,.T.) ;
#3220 = ORIENTED_EDGE('',*,*,#2268,.T.) ;
#3221 = ORIENTED_EDGE('',*,*,#2266,.F.) ;
#3222 = ORIENTED_EDGE('',*,*,#2269,.F.) ;
#3223 = ORIENTED_EDGE('',*,*,#2270,.T.) ;
#3224 = ORIENTED_EDGE('',*,*,#2271,.T.) ;
#3225 = ORIENTED_EDGE('',*,*,#2270,.F.) ;
#3226 = ORIENTED_EDGE('',*,*,#2272,.F.) ;
#3227 = ORIENTED_EDGE('',*,*,#2273,.F.) ;
#3228 = ORIENTED_EDGE('',*,*,#2274,.T.) ;
#3229 = ORIENTED_EDGE('',*,*,#2275,.T.) ;
#3230 = ORIENTED_EDGE('',*,*,#2276,.T.) ;
#3231 = ORIENTED_EDGE('',*,*,#2274,.F.) ;
#3232 = ORIENTED_EDGE('',*,*,#2277,.T.) ;
#3233 = ORIENTED_EDGE('',*,*,#2278,.T.) ;
#3234 = ORIENTED_EDGE('',*,*,#2279,.F.) ;
#3235 = ORIENTED_EDGE('',*,*,#2280,.F.) ;
#3236 = ORIENTED_EDGE('',*,*,#2278,.F.) ;
#3237 = ORIENTED_EDGE('',*,*,#2281,.T.) ;
#3238 = ORIENTED_EDGE('',*,*,#2282,.F.) ;
#3239 = ORIENTED_EDGE('',*,*,#2283,.F.) ;
#3240 = ORIENTED_EDGE('',*,*,#2284,.T.) ;
#3241 = ORIENTED_EDGE('',*,*,#2285,.T.) ;
#3242 = ORIENTED_EDGE('',*,*,#2286,.T.) ;
#3243 = ORIENTED_EDGE('',*,*,#2284,.F.) ;
#3244 = ORIENTED_EDGE('',*,*,#2287,.F.) ;
#3245 = ORIENTED_EDGE('',*,*,#2288,.F.) ;
#3246 = ORIENTED_EDGE('',*,*,#2289,.T.) ;
#3247 = ORIENTED_EDGE('',*,*,#2290,.T.) ;
#3248 = ORIENTED_EDGE('',*,*,#2289,.F.) ;
#3249 = ORIENTED_EDGE('',*,*,#2291,.F.) ;
#3250 = ORIENTED_EDGE('',*,*,#2292,.T.) ;
#3251 = ORIENTED_EDGE('',*,*,#2293,.T.) ;
#3252 = ORIENTED_EDGE('',*,*,#2292,.F.) ;
#3253 = ORIENTED_EDGE('',*,*,#2294,.F.) ;
#3254 = ORIENTED_EDGE('',*,*,#2295,.F.) ;
#3255 = ORIENTED_EDGE('',*,*,#2296,.T.) ;
#3256 = ORIENTED_EDGE('',*,*,#2297,.T.) ;
#3257 = ORIENTED_EDGE('',*,*,#2298,.T.) ;
#3258 = ORIENTED_EDGE('',*,*,#2296,.F.) ;
#3259 = ORIENTED_EDGE('',*,*,#2282,.T.) ;
#3260 = ORIENTED_EDGE('',*,*,#2283,.T.) ;
#3261 = ORIENTED_EDGE('',*,*,#2299,.T.) ;
#3262 = ORIENTED_EDGE('',*,*,#2267,.F.) ;
#3263 = ORIENTED_EDGE('',*,*,#2268,.F.) ;
#3264 = ORIENTED_EDGE('',*,*,#2299,.F.) ;
#3265 = ORIENTED_EDGE('',*,*,#2265,.T.) ;
#3266 = ORIENTED_EDGE('',*,*,#2300,.T.) ;
#3267 = ORIENTED_EDGE('',*,*,#2271,.F.) ;
#3268 = ORIENTED_EDGE('',*,*,#2300,.F.) ;
#3269 = ORIENTED_EDGE('',*,*,#2269,.T.) ;
#3270 = ORIENTED_EDGE('',*,*,#2301,.T.) ;
#3271 = ORIENTED_EDGE('',*,*,#2275,.F.) ;
#3272 = ORIENTED_EDGE('',*,*,#2276,.F.) ;
#3273 = ORIENTED_EDGE('',*,*,#2301,.F.) ;
#3274 = ORIENTED_EDGE('',*,*,#2272,.T.) ;
#3275 = ORIENTED_EDGE('',*,*,#2273,.T.) ;
#3276 = ORIENTED_EDGE('',*,*,#2302,.T.) ;
#3277 = ORIENTED_EDGE('',*,*,#2281,.F.) ;
#3278 = ORIENTED_EDGE('',*,*,#2277,.F.) ;
#3279 = ORIENTED_EDGE('',*,*,#2302,.F.) ;
#3280 = ORIENTED_EDGE('',*,*,#2286,.F.) ;
#3281 = ORIENTED_EDGE('',*,*,#2303,.T.) ;
#3282 = ORIENTED_EDGE('',*,*,#2287,.T.) ;
#3283 = ORIENTED_EDGE('',*,*,#2288,.T.) ;
#3284 = ORIENTED_EDGE('',*,*,#2303,.F.) ;
#3285 = ORIENTED_EDGE('',*,*,#2285,.F.) ;
#3286 = ORIENTED_EDGE('',*,*,#2290,.F.) ;
#3287 = ORIENTED_EDGE('',*,*,#2304,.T.) ;
#3288 = ORIENTED_EDGE('',*,*,#2291,.T.) ;
#3289 = ORIENTED_EDGE('',*,*,#2304,.F.) ;
#3290 = ORIENTED_EDGE('',*,*,#2293,.F.) ;
#3291 = ORIENTED_EDGE('',*,*,#2305,.T.) ;
#3292 = ORIENTED_EDGE('',*,*,#2294,.T.) ;
#3293 = ORIENTED_EDGE('',*,*,#2295,.T.) ;
#3294 = ORIENTED_EDGE('',*,*,#2305,.F.) ;
#3295 = ORIENTED_EDGE('',*,*,#2298,.F.) ;
#3296 = ORIENTED_EDGE('',*,*,#2306,.T.) ;
#3297 = ORIENTED_EDGE('',*,*,#2279,.T.) ;
#3298 = ORIENTED_EDGE('',*,*,#2280,.T.) ;
#3299 = ORIENTED_EDGE('',*,*,#2306,.F.) ;
#3300 = ORIENTED_EDGE('',*,*,#2297,.F.) ;
#3301 = TOROIDAL_SURFACE('',#3946,42.1235909466484,7.1235909466484) ;
#3302 = TOROIDAL_SURFACE('',#3951,42.1235909466484,7.27359094664848) ;
#3303 = TOROIDAL_SURFACE('',#3959,46.1132125609321,12.6169576826623) ;
#3304 = TOROIDAL_SURFACE('',#3968,46.1132125609321,12.7669576826623) ;
#3305 = TOROIDAL_SURFACE('',#3974,35.75,0.349999999999999) ;
#3306 = TOROIDAL_SURFACE('',#3978,35.75,0.349999999999999) ;
#3307 = TOROIDAL_SURFACE('',#3982,35.75,0.349999999999999) ;
#3308 = TOROIDAL_SURFACE('',#3986,35.75,0.349999999999999) ;
#3309 = TOROIDAL_SURFACE('',#3990,35.75,0.349999999999999) ;
#3310 = TOROIDAL_SURFACE('',#3994,35.4268144613668,0.349999999999999) ;
#3311 = TOROIDAL_SURFACE('',#3998,33.4268144613668,0.349999999999999) ;
#3312 = TOROIDAL_SURFACE('',#4002,31.4268144613668,0.349999999999999) ;
#3313 = TOROIDAL_SURFACE('',#4006,29.4268144613668,0.349999999999999) ;
#3314 = TOROIDAL_SURFACE('',#4010,27.4268144613668,0.349999999999999) ;
#3315 = TOROIDAL_SURFACE('',#4014,25.4268144613668,0.349999999999999) ;
#3316 = TOROIDAL_SURFACE('',#4018,23.4268144613668,0.349999999999999) ;
#3317 = TOROIDAL_SURFACE('',#4022,21.4268144613668,0.349999999999999) ;
#3318 = TOROIDAL_SURFACE('',#4026,19.4268144613668,0.349999999999999) ;
#3319 = TOROIDAL_SURFACE('',#4030,17.4268144613668,0.349999999999999) ;
#3320 = TOROIDAL_SURFACE('',#4034,15.4268144613668,0.349999999999999) ;
#3321 = TOROIDAL_SURFACE('',#4038,13.4268144613668,0.349999999999999) ;
#3322 = TOROIDAL_SURFACE('',#4042,11.4268144613668,0.349999999999999) ;
#3323 = TOROIDAL_SURFACE('',#4046,9.42681446136679,0.349999999999999) ;
#3324 = TOROIDAL_SURFACE('',#4050,7.42681446136678,0.349999999999999) ;
#3325 = TOROIDAL_SURFACE('',#4054,5.42681446136678,0.349999999999999) ;
#3326 = TOROIDAL_SURFACE('',#4058,3.42681446136678,0.349999999999999) ;
#3327 = TOROIDAL_SURFACE('',#4233,1.5,0.6) ;
#3328 = TOROIDAL_SURFACE('',#4238,2.,0.6) ;
#3329 = TOROIDAL_SURFACE('',#4242,2.,0.6) ;
#3330 = TOROIDAL_SURFACE('',#4248,1.,0.6) ;
#3331 = TOROIDAL_SURFACE('',#4254,1.,0.599999999999999) ;
#3332 = TOROIDAL_SURFACE('',#4260,1.5,0.6) ;
#3333 = TOROIDAL_SURFACE('',#4265,2.,0.6) ;
#3334 = TOROIDAL_SURFACE('',#4269,2.,0.6) ;
#3335 = TOROIDAL_SURFACE('',#4284,1.5,0.6) ;
#3336 = TOROIDAL_SURFACE('',#4289,2.,0.6) ;
#3337 = TOROIDAL_SURFACE('',#4293,2.,0.6) ;
#3338 = TOROIDAL_SURFACE('',#4299,1.,0.6) ;
#3339 = TOROIDAL_SURFACE('',#4305,1.,0.599999999999999) ;
#3340 = TOROIDAL_SURFACE('',#4311,1.5,0.6) ;
#3341 = TOROIDAL_SURFACE('',#4316,2.,0.6) ;
#3342 = TOROIDAL_SURFACE('',#4320,2.,0.6) ;
#3343 = TOROIDAL_SURFACE('',#4335,1.5,0.6) ;
#3344 = TOROIDAL_SURFACE('',#4340,2.,0.6) ;
#3345 = TOROIDAL_SURFACE('',#4344,2.,0.6) ;
#3346 = TOROIDAL_SURFACE('',#4350,1.,0.6) ;
#3347 = TOROIDAL_SURFACE('',#4356,1.,0.599999999999999) ;
#3348 = TOROIDAL_SURFACE('',#4362,1.5,0.6) ;
#3349 = TOROIDAL_SURFACE('',#4367,2.,0.6) ;
#3350 = TOROIDAL_SURFACE('',#4371,2.,0.6) ;
#3351 = TOROIDAL_SURFACE('',#4386,1.5,0.6) ;
#3352 = TOROIDAL_SURFACE('',#4391,2.,0.6) ;
#3353 = TOROIDAL_SURFACE('',#4395,2.,0.6) ;
#3354 = TOROIDAL_SURFACE('',#4401,1.,0.6) ;
#3355 = TOROIDAL_SURFACE('',#4407,1.,0.599999999999999) ;
#3356 = TOROIDAL_SURFACE('',#4413,1.5,0.6) ;
#3357 = TOROIDAL_SURFACE('',#4418,2.,0.6) ;
#3358 = TOROIDAL_SURFACE('',#4422,2.,0.6) ;
#3359 = ADVANCED_FACE('',(#851),#3301,.F.) ;
#3360 = ADVANCED_FACE('',(#852),#3302,.T.) ;
#3361 = ADVANCED_FACE('',(#853),#848,.T.) ;
#3362 = ADVANCED_FACE('',(#854,#468),#477,.F.) ;
#3363 = ADVANCED_FACE('',(#855),#3303,.F.) ;
#3364 = ADVANCED_FACE('',(#856),#849,.T.) ;
#3365 = ADVANCED_FACE('',(#857),#3304,.T.) ;
#3366 = ADVANCED_FACE('',(#858),#850,.F.) ;
#3367 = ADVANCED_FACE('',(#859),#3305,.T.) ;
#3368 = ADVANCED_FACE('',(#860),#3306,.T.) ;
#3369 = ADVANCED_FACE('',(#861),#3307,.T.) ;
#3370 = ADVANCED_FACE('',(#862),#3308,.T.) ;
#3371 = ADVANCED_FACE('',(#863),#3309,.T.) ;
#3372 = ADVANCED_FACE('',(#864),#3310,.T.) ;
#3373 = ADVANCED_FACE('',(#865),#3311,.T.) ;
#3374 = ADVANCED_FACE('',(#866),#3312,.T.) ;
#3375 = ADVANCED_FACE('',(#867),#3313,.T.) ;
#3376 = ADVANCED_FACE('',(#868),#3314,.T.) ;
#3377 = ADVANCED_FACE('',(#869),#3315,.T.) ;
#3378 = ADVANCED_FACE('',(#870),#3316,.T.) ;
#3379 = ADVANCED_FACE('',(#871),#3317,.T.) ;
#3380 = ADVANCED_FACE('',(#872),#3318,.T.) ;
#3381 = ADVANCED_FACE('',(#873),#3319,.T.) ;
#3382 = ADVANCED_FACE('',(#874),#3320,.T.) ;
#3383 = ADVANCED_FACE('',(#875),#3321,.T.) ;
#3384 = ADVANCED_FACE('',(#876),#3322,.T.) ;
#3385 = ADVANCED_FACE('',(#877),#3323,.T.) ;
#3386 = ADVANCED_FACE('',(#878),#3324,.T.) ;
#3387 = ADVANCED_FACE('',(#879),#3325,.T.) ;
#3388 = ADVANCED_FACE('',(#880),#3326,.T.) ;
#3389 = ADVANCED_FACE('',(#881,#469,#470,#471,#472),#129,.T.) ;
#3390 = ADVANCED_FACE('',(#882),#478,.F.) ;
#3391 = ADVANCED_FACE('',(#883),#31,.T.) ;
#3392 = ADVANCED_FACE('',(#884),#32,.T.) ;
#3393 = ADVANCED_FACE('',(#885),#130,.T.) ;
#3394 = ADVANCED_FACE('',(#886),#131,.T.) ;
#3395 = ADVANCED_FACE('',(#887),#132,.T.) ;
#3396 = ADVANCED_FACE('',(#888),#479,.T.) ;
#3397 = ADVANCED_FACE('',(#889),#480,.F.) ;
#3398 = ADVANCED_FACE('',(#890),#33,.F.) ;
#3399 = ADVANCED_FACE('',(#891),#34,.F.) ;
#3400 = ADVANCED_FACE('',(#892),#481,.F.) ;
#3401 = ADVANCED_FACE('',(#893),#35,.T.) ;
#3402 = ADVANCED_FACE('',(#894),#36,.T.) ;
#3403 = ADVANCED_FACE('',(#895),#133,.T.) ;
#3404 = ADVANCED_FACE('',(#896),#134,.T.) ;
#3405 = ADVANCED_FACE('',(#897),#135,.T.) ;
#3406 = ADVANCED_FACE('',(#898),#482,.T.) ;
#3407 = ADVANCED_FACE('',(#899),#37,.F.) ;
#3408 = ADVANCED_FACE('',(#900),#38,.F.) ;
#3409 = ADVANCED_FACE('',(#901),#483,.T.) ;
#3410 = ADVANCED_FACE('',(#902),#484,.F.) ;
#3411 = ADVANCED_FACE('',(#903),#39,.T.) ;
#3412 = ADVANCED_FACE('',(#904),#40,.T.) ;
#3413 = ADVANCED_FACE('',(#905),#136,.T.) ;
#3414 = ADVANCED_FACE('',(#906),#137,.T.) ;
#3415 = ADVANCED_FACE('',(#907),#138,.T.) ;
#3416 = ADVANCED_FACE('',(#908),#485,.T.) ;
#3417 = ADVANCED_FACE('',(#909),#41,.F.) ;
#3418 = ADVANCED_FACE('',(#910),#42,.F.) ;
#3419 = ADVANCED_FACE('',(#911),#486,.F.) ;
#3420 = ADVANCED_FACE('',(#912),#43,.T.) ;
#3421 = ADVANCED_FACE('',(#913),#44,.T.) ;
#3422 = ADVANCED_FACE('',(#914),#139,.T.) ;
#3423 = ADVANCED_FACE('',(#915),#140,.T.) ;
#3424 = ADVANCED_FACE('',(#916),#141,.T.) ;
#3425 = ADVANCED_FACE('',(#917),#487,.T.) ;
#3426 = ADVANCED_FACE('',(#918),#45,.F.) ;
#3427 = ADVANCED_FACE('',(#919),#46,.F.) ;
#3428 = ADVANCED_FACE('',(#920),#488,.F.) ;
#3429 = ADVANCED_FACE('',(#921),#47,.T.) ;
#3430 = ADVANCED_FACE('',(#922),#48,.T.) ;
#3431 = ADVANCED_FACE('',(#923),#142,.T.) ;
#3432 = ADVANCED_FACE('',(#924),#143,.T.) ;
#3433 = ADVANCED_FACE('',(#925),#144,.T.) ;
#3434 = ADVANCED_FACE('',(#926),#489,.T.) ;
#3435 = ADVANCED_FACE('',(#927),#49,.F.) ;
#3436 = ADVANCED_FACE('',(#928),#50,.F.) ;
#3437 = ADVANCED_FACE('',(#929),#145,.F.) ;
#3438 = ADVANCED_FACE('',(#930),#146,.T.) ;
#3439 = ADVANCED_FACE('',(#931,#473),#490,.T.) ;
#3440 = ADVANCED_FACE('',(#932,#474),#491,.F.) ;
#3441 = ADVANCED_FACE('',(#933),#492,.F.) ;
#3442 = ADVANCED_FACE('',(#934),#493,.F.) ;
#3443 = ADVANCED_FACE('',(#935),#494,.F.) ;
#3444 = ADVANCED_FACE('',(#936),#495,.F.) ;
#3445 = ADVANCED_FACE('',(#937),#496,.T.) ;
#3446 = ADVANCED_FACE('',(#938),#497,.F.) ;
#3447 = ADVANCED_FACE('',(#939),#147,.T.) ;
#3448 = ADVANCED_FACE('',(#940),#148,.T.) ;
#3449 = ADVANCED_FACE('',(#941),#149,.T.) ;
#3450 = ADVANCED_FACE('',(#942),#150,.T.) ;
#3451 = ADVANCED_FACE('',(#943),#151,.F.) ;
#3452 = ADVANCED_FACE('',(#944,#475),#498,.F.) ;
#3453 = ADVANCED_FACE('',(#945,#476),#499,.T.) ;
#3454 = ADVANCED_FACE('',(#946),#500,.F.) ;
#3455 = ADVANCED_FACE('',(#947),#501,.F.) ;
#3456 = ADVANCED_FACE('',(#948),#502,.F.) ;
#3457 = ADVANCED_FACE('',(#949),#503,.F.) ;
#3458 = ADVANCED_FACE('',(#950),#504,.T.) ;
#3459 = ADVANCED_FACE('',(#951),#505,.F.) ;
#3460 = ADVANCED_FACE('',(#952),#152,.T.) ;
#3461 = ADVANCED_FACE('',(#953),#153,.F.) ;
#3462 = ADVANCED_FACE('',(#954),#506,.F.) ;
#3463 = ADVANCED_FACE('',(#955),#507,.F.) ;
#3464 = ADVANCED_FACE('',(#956),#508,.F.) ;
#3465 = ADVANCED_FACE('',(#957),#509,.T.) ;
#3466 = ADVANCED_FACE('',(#958),#510,.F.) ;
#3467 = ADVANCED_FACE('',(#959),#511,.T.) ;
#3468 = ADVANCED_FACE('',(#960),#512,.F.) ;
#3469 = ADVANCED_FACE('',(#961),#154,.T.) ;
#3470 = ADVANCED_FACE('',(#962),#155,.F.) ;
#3471 = ADVANCED_FACE('',(#963),#513,.F.) ;
#3472 = ADVANCED_FACE('',(#964),#514,.F.) ;
#3473 = ADVANCED_FACE('',(#965),#515,.F.) ;
#3474 = ADVANCED_FACE('',(#966),#516,.T.) ;
#3475 = ADVANCED_FACE('',(#967),#517,.F.) ;
#3476 = ADVANCED_FACE('',(#968),#518,.T.) ;
#3477 = ADVANCED_FACE('',(#969),#519,.F.) ;
#3478 = ADVANCED_FACE('',(#970),#156,.T.) ;
#3479 = ADVANCED_FACE('',(#971),#157,.F.) ;
#3480 = ADVANCED_FACE('',(#972),#520,.F.) ;
#3481 = ADVANCED_FACE('',(#973),#521,.F.) ;
#3482 = ADVANCED_FACE('',(#974),#522,.F.) ;
#3483 = ADVANCED_FACE('',(#975),#523,.T.) ;
#3484 = ADVANCED_FACE('',(#976),#524,.F.) ;
#3485 = ADVANCED_FACE('',(#977),#525,.T.) ;
#3486 = ADVANCED_FACE('',(#978),#526,.F.) ;
#3487 = ADVANCED_FACE('',(#979),#158,.T.) ;
#3488 = ADVANCED_FACE('',(#980),#159,.F.) ;
#3489 = ADVANCED_FACE('',(#981),#527,.F.) ;
#3490 = ADVANCED_FACE('',(#982),#528,.F.) ;
#3491 = ADVANCED_FACE('',(#983),#529,.F.) ;
#3492 = ADVANCED_FACE('',(#984),#530,.T.) ;
#3493 = ADVANCED_FACE('',(#985),#531,.F.) ;
#3494 = ADVANCED_FACE('',(#986),#3327,.T.) ;
#3495 = ADVANCED_FACE('',(#987),#3328,.T.) ;
#3496 = ADVANCED_FACE('',(#988),#3329,.T.) ;
#3497 = ADVANCED_FACE('',(#989),#3330,.T.) ;
#3498 = ADVANCED_FACE('',(#990),#3331,.T.) ;
#3499 = ADVANCED_FACE('',(#991),#3332,.T.) ;
#3500 = ADVANCED_FACE('',(#992),#3333,.T.) ;
#3501 = ADVANCED_FACE('',(#993),#3334,.T.) ;
#3502 = ADVANCED_FACE('',(#994),#160,.T.) ;
#3503 = ADVANCED_FACE('',(#995),#161,.T.) ;
#3504 = ADVANCED_FACE('',(#996),#162,.T.) ;
#3505 = ADVANCED_FACE('',(#997),#163,.T.) ;
#3506 = ADVANCED_FACE('',(#998),#164,.T.) ;
#3507 = ADVANCED_FACE('',(#999),#165,.T.) ;
#3508 = ADVANCED_FACE('',(#1000),#166,.T.) ;
#3509 = ADVANCED_FACE('',(#1001),#167,.T.) ;
#3510 = ADVANCED_FACE('',(#1002),#3335,.T.) ;
#3511 = ADVANCED_FACE('',(#1003),#3336,.T.) ;
#3512 = ADVANCED_FACE('',(#1004),#3337,.T.) ;
#3513 = ADVANCED_FACE('',(#1005),#3338,.T.) ;
#3514 = ADVANCED_FACE('',(#1006),#3339,.T.) ;
#3515 = ADVANCED_FACE('',(#1007),#3340,.T.) ;
#3516 = ADVANCED_FACE('',(#1008),#3341,.T.) ;
#3517 = ADVANCED_FACE('',(#1009),#3342,.T.) ;
#3518 = ADVANCED_FACE('',(#1010),#168,.T.) ;
#3519 = ADVANCED_FACE('',(#1011),#169,.T.) ;
#3520 = ADVANCED_FACE('',(#1012),#170,.T.) ;
#3521 = ADVANCED_FACE('',(#1013),#171,.T.) ;
#3522 = ADVANCED_FACE('',(#1014),#172,.T.) ;
#3523 = ADVANCED_FACE('',(#1015),#173,.T.) ;
#3524 = ADVANCED_FACE('',(#1016),#174,.T.) ;
#3525 = ADVANCED_FACE('',(#1017),#175,.T.) ;
#3526 = ADVANCED_FACE('',(#1018),#3343,.T.) ;
#3527 = ADVANCED_FACE('',(#1019),#3344,.T.) ;
#3528 = ADVANCED_FACE('',(#1020),#3345,.T.) ;
#3529 = ADVANCED_FACE('',(#1021),#3346,.T.) ;
#3530 = ADVANCED_FACE('',(#1022),#3347,.T.) ;
#3531 = ADVANCED_FACE('',(#1023),#3348,.T.) ;
#3532 = ADVANCED_FACE('',(#1024),#3349,.T.) ;
#3533 = ADVANCED_FACE('',(#1025),#3350,.T.) ;
#3534 = ADVANCED_FACE('',(#1026),#176,.T.) ;
#3535 = ADVANCED_FACE('',(#1027),#177,.T.) ;
#3536 = ADVANCED_FACE('',(#1028),#178,.T.) ;
#3537 = ADVANCED_FACE('',(#1029),#179,.T.) ;
#3538 = ADVANCED_FACE('',(#1030),#180,.T.) ;
#3539 = ADVANCED_FACE('',(#1031),#181,.T.) ;
#3540 = ADVANCED_FACE('',(#1032),#182,.T.) ;
#3541 = ADVANCED_FACE('',(#1033),#183,.T.) ;
#3542 = ADVANCED_FACE('',(#1034),#3351,.T.) ;
#3543 = ADVANCED_FACE('',(#1035),#3352,.T.) ;
#3544 = ADVANCED_FACE('',(#1036),#3353,.T.) ;
#3545 = ADVANCED_FACE('',(#1037),#3354,.T.) ;
#3546 = ADVANCED_FACE('',(#1038),#3355,.T.) ;
#3547 = ADVANCED_FACE('',(#1039),#3356,.T.) ;
#3548 = ADVANCED_FACE('',(#1040),#3357,.T.) ;
#3549 = ADVANCED_FACE('',(#1041),#3358,.T.) ;
#3550 = ADVANCED_FACE('',(#1042),#184,.T.) ;
#3551 = ADVANCED_FACE('',(#1043),#185,.T.) ;
#3552 = ADVANCED_FACE('',(#1044),#186,.T.) ;
#3553 = ADVANCED_FACE('',(#1045),#187,.T.) ;
#3554 = ADVANCED_FACE('',(#1046),#188,.T.) ;
#3555 = ADVANCED_FACE('',(#1047),#189,.T.) ;
#3556 = ADVANCED_FACE('',(#1048),#190,.T.) ;
#3557 = ADVANCED_FACE('',(#1049),#191,.T.) ;
#3558 = CLOSED_SHELL('',(#3359,#3360,#3361,#3362)) ;
#3559 = CLOSED_SHELL('',(#3363,#3364,#3365,#3366)) ;
#3560 = CLOSED_SHELL('',(#3367)) ;
#3561 = CLOSED_SHELL('',(#3368)) ;
#3562 = CLOSED_SHELL('',(#3369)) ;
#3563 = CLOSED_SHELL('',(#3370)) ;
#3564 = CLOSED_SHELL('',(#3371)) ;
#3565 = CLOSED_SHELL('',(#3372)) ;
#3566 = CLOSED_SHELL('',(#3373)) ;
#3567 = CLOSED_SHELL('',(#3374)) ;
#3568 = CLOSED_SHELL('',(#3375)) ;
#3569 = CLOSED_SHELL('',(#3376)) ;
#3570 = CLOSED_SHELL('',(#3377)) ;
#3571 = CLOSED_SHELL('',(#3378)) ;
#3572 = CLOSED_SHELL('',(#3379)) ;
#3573 = CLOSED_SHELL('',(#3380)) ;
#3574 = CLOSED_SHELL('',(#3381)) ;
#3575 = CLOSED_SHELL('',(#3382)) ;
#3576 = CLOSED_SHELL('',(#3383)) ;
#3577 = CLOSED_SHELL('',(#3384)) ;
#3578 = CLOSED_SHELL('',(#3385)) ;
#3579 = CLOSED_SHELL('',(#3386)) ;
#3580 = CLOSED_SHELL('',(#3387)) ;
#3581 = CLOSED_SHELL('',(#3388)) ;
#3582 = CLOSED_SHELL('',(#3389,#3390,#3391,#3392,#3393,#3394,#3395,#3396,
#3397,#3398,#3399,#3400,#3401,#3402,#3403,#3404,#3405,#3406,#3407,#3408,
#3409,#3410,#3411,#3412,#3413,#3414,#3415,#3416,#3417,#3418,#3419,#3420,
#3421,#3422,#3423,#3424,#3425,#3426,#3427,#3428,#3429,#3430,#3431,#3432,
#3433,#3434,#3435,#3436)) ;
#3583 = CLOSED_SHELL('',(#3437,#3438,#3439,#3440)) ;
#3584 = CLOSED_SHELL('',(#3441,#3442,#3443,#3444,#3445,#3446,#3447,#3448,
#3449,#3450)) ;
#3585 = CLOSED_SHELL('',(#3451,#3452,#3453,#3454,#3455,#3456,#3457,#3458,
#3459,#3460,#3461,#3462,#3463,#3464,#3465,#3466,#3467,#3468,#3469,#3470,
#3471,#3472,#3473,#3474,#3475,#3476,#3477,#3478,#3479,#3480,#3481,#3482,
#3483,#3484,#3485,#3486,#3487,#3488,#3489,#3490,#3491,#3492,#3493)) ;
#3586 = CLOSED_SHELL('',(#3494,#3495,#3496,#3497,#3498,#3499,#3500,#3501,
#3502,#3503,#3504,#3505,#3506,#3507,#3508,#3509)) ;
#3587 = CLOSED_SHELL('',(#3510,#3511,#3512,#3513,#3514,#3515,#3516,#3517,
#3518,#3519,#3520,#3521,#3522,#3523,#3524,#3525)) ;
#3588 = CLOSED_SHELL('',(#3526,#3527,#3528,#3529,#3530,#3531,#3532,#3533,
#3534,#3535,#3536,#3537,#3538,#3539,#3540,#3541)) ;
#3589 = CLOSED_SHELL('',(#3542,#3543,#3544,#3545,#3546,#3547,#3548,#3549,
#3550,#3551,#3552,#3553,#3554,#3555,#3556,#3557)) ;
#3590 = DERIVED_UNIT_ELEMENT(#3654,1.) ;
#3591 = DERIVED_UNIT_ELEMENT(#10336,-3.) ;
#3592 = DERIVED_UNIT_ELEMENT(#3654,1.) ;
#3593 = DERIVED_UNIT_ELEMENT(#10336,-3.) ;
#3594 = DERIVED_UNIT_ELEMENT(#3654,1.) ;
#3595 = DERIVED_UNIT_ELEMENT(#10336,-3.) ;
#3596 = DERIVED_UNIT_ELEMENT(#3654,1.) ;
#3597 = DERIVED_UNIT_ELEMENT(#10336,-3.) ;
#3598 = DERIVED_UNIT_ELEMENT(#3654,1.) ;
#3599 = DERIVED_UNIT_ELEMENT(#10336,-3.) ;
#3600 = DERIVED_UNIT_ELEMENT(#3654,1.) ;
#3601 = DERIVED_UNIT_ELEMENT(#10336,-3.) ;
#3602 = DERIVED_UNIT_ELEMENT(#3654,1.) ;
#3603 = DERIVED_UNIT_ELEMENT(#10336,-3.) ;
#3604 = DERIVED_UNIT_ELEMENT(#3654,1.) ;
#3605 = DERIVED_UNIT_ELEMENT(#10336,-3.) ;
#3606 = DERIVED_UNIT_ELEMENT(#3654,1.) ;
#3607 = DERIVED_UNIT_ELEMENT(#10336,-3.) ;
#3608 = DERIVED_UNIT_ELEMENT(#3654,1.) ;
#3609 = DERIVED_UNIT_ELEMENT(#10336,-3.) ;
#3610 = DERIVED_UNIT_ELEMENT(#3654,1.) ;
#3611 = DERIVED_UNIT_ELEMENT(#10336,-3.) ;
#3612 = DERIVED_UNIT_ELEMENT(#3654,1.) ;
#3613 = DERIVED_UNIT_ELEMENT(#10336,-3.) ;
#3614 = DERIVED_UNIT_ELEMENT(#3654,1.) ;
#3615 = DERIVED_UNIT_ELEMENT(#10336,-3.) ;
#3616 = DERIVED_UNIT_ELEMENT(#3654,1.) ;
#3617 = DERIVED_UNIT_ELEMENT(#10336,-3.) ;
#3618 = DERIVED_UNIT_ELEMENT(#3654,1.) ;
#3619 = DERIVED_UNIT_ELEMENT(#10336,-3.) ;
#3620 = DERIVED_UNIT_ELEMENT(#3654,1.) ;
#3621 = DERIVED_UNIT_ELEMENT(#10336,-3.) ;
#3622 = DERIVED_UNIT_ELEMENT(#3654,1.) ;
#3623 = DERIVED_UNIT_ELEMENT(#10336,-3.) ;
#3624 = DERIVED_UNIT_ELEMENT(#3654,1.) ;
#3625 = DERIVED_UNIT_ELEMENT(#10336,-3.) ;
#3626 = DERIVED_UNIT_ELEMENT(#3654,1.) ;
#3627 = DERIVED_UNIT_ELEMENT(#10336,-3.) ;
#3628 = DERIVED_UNIT_ELEMENT(#3654,1.) ;
#3629 = DERIVED_UNIT_ELEMENT(#10336,-3.) ;
#3630 = DERIVED_UNIT_ELEMENT(#3654,1.) ;
#3631 = DERIVED_UNIT_ELEMENT(#10336,-3.) ;
#3632 = DERIVED_UNIT_ELEMENT(#3654,1.) ;
#3633 = DERIVED_UNIT_ELEMENT(#10336,-3.) ;
#3634 = DERIVED_UNIT_ELEMENT(#3654,1.) ;
#3635 = DERIVED_UNIT_ELEMENT(#10336,-3.) ;
#3636 = DERIVED_UNIT_ELEMENT(#3654,1.) ;
#3637 = DERIVED_UNIT_ELEMENT(#10336,-3.) ;
#3638 = DERIVED_UNIT_ELEMENT(#3654,1.) ;
#3639 = DERIVED_UNIT_ELEMENT(#10336,-3.) ;
#3640 = DERIVED_UNIT_ELEMENT(#3654,1.) ;
#3641 = DERIVED_UNIT_ELEMENT(#10336,-3.) ;
#3642 = DERIVED_UNIT_ELEMENT(#3654,1.) ;
#3643 = DERIVED_UNIT_ELEMENT(#10336,-3.) ;
#3644 = DERIVED_UNIT_ELEMENT(#3654,1.) ;
#3645 = DERIVED_UNIT_ELEMENT(#10336,-3.) ;
#3646 = DERIVED_UNIT_ELEMENT(#3654,1.) ;
#3647 = DERIVED_UNIT_ELEMENT(#10336,-3.) ;
#3648 = DERIVED_UNIT_ELEMENT(#3654,1.) ;
#3649 = DERIVED_UNIT_ELEMENT(#10336,-3.) ;
#3650 = DERIVED_UNIT_ELEMENT(#3654,1.) ;
#3651 = DERIVED_UNIT_ELEMENT(#10336,-3.) ;
#3652 = DERIVED_UNIT_ELEMENT(#3654,1.) ;
#3653 = DERIVED_UNIT_ELEMENT(#10336,-3.) ;
#3654 = (
MASS_UNIT()
NAMED_UNIT(*)
SI_UNIT(.KILO.,.GRAM.)
) ;
#3655 = DERIVED_UNIT((#3590,#3591)) ;
#3656 = DERIVED_UNIT((#3592,#3593)) ;
#3657 = DERIVED_UNIT((#3594,#3595)) ;
#3658 = DERIVED_UNIT((#3596,#3597)) ;
#3659 = DERIVED_UNIT((#3598,#3599)) ;
#3660 = DERIVED_UNIT((#3600,#3601)) ;
#3661 = DERIVED_UNIT((#3602,#3603)) ;
#3662 = DERIVED_UNIT((#3604,#3605)) ;
#3663 = DERIVED_UNIT((#3606,#3607)) ;
#3664 = DERIVED_UNIT((#3608,#3609)) ;
#3665 = DERIVED_UNIT((#3610,#3611)) ;
#3666 = DERIVED_UNIT((#3612,#3613)) ;
#3667 = DERIVED_UNIT((#3614,#3615)) ;
#3668 = DERIVED_UNIT((#3616,#3617)) ;
#3669 = DERIVED_UNIT((#3618,#3619)) ;
#3670 = DERIVED_UNIT((#3620,#3621)) ;
#3671 = DERIVED_UNIT((#3622,#3623)) ;
#3672 = DERIVED_UNIT((#3624,#3625)) ;
#3673 = DERIVED_UNIT((#3626,#3627)) ;
#3674 = DERIVED_UNIT((#3628,#3629)) ;
#3675 = DERIVED_UNIT((#3630,#3631)) ;
#3676 = DERIVED_UNIT((#3632,#3633)) ;
#3677 = DERIVED_UNIT((#3634,#3635)) ;
#3678 = DERIVED_UNIT((#3636,#3637)) ;
#3679 = DERIVED_UNIT((#3638,#3639)) ;
#3680 = DERIVED_UNIT((#3640,#3641)) ;
#3681 = DERIVED_UNIT((#3642,#3643)) ;
#3682 = DERIVED_UNIT((#3644,#3645)) ;
#3683 = DERIVED_UNIT((#3646,#3647)) ;
#3684 = DERIVED_UNIT((#3648,#3649)) ;
#3685 = DERIVED_UNIT((#3650,#3651)) ;
#3686 = DERIVED_UNIT((#3652,#3653)) ;
#3687 = MEASURE_REPRESENTATION_ITEM('density measure',
POSITIVE_RATIO_MEASURE(7850.),#3655) ;
#3688 = MEASURE_REPRESENTATION_ITEM('density measure',
POSITIVE_RATIO_MEASURE(7850.),#3656) ;
#3689 = MEASURE_REPRESENTATION_ITEM('density measure',
POSITIVE_RATIO_MEASURE(7850.),#3657) ;
#3690 = MEASURE_REPRESENTATION_ITEM('density measure',
POSITIVE_RATIO_MEASURE(7850.),#3658) ;
#3691 = MEASURE_REPRESENTATION_ITEM('density measure',
POSITIVE_RATIO_MEASURE(7850.),#3659) ;
#3692 = MEASURE_REPRESENTATION_ITEM('density measure',
POSITIVE_RATIO_MEASURE(7850.),#3660) ;
#3693 = MEASURE_REPRESENTATION_ITEM('density measure',
POSITIVE_RATIO_MEASURE(7850.),#3661) ;
#3694 = MEASURE_REPRESENTATION_ITEM('density measure',
POSITIVE_RATIO_MEASURE(7850.),#3662) ;
#3695 = MEASURE_REPRESENTATION_ITEM('density measure',
POSITIVE_RATIO_MEASURE(7850.),#3663) ;
#3696 = MEASURE_REPRESENTATION_ITEM('density measure',
POSITIVE_RATIO_MEASURE(7850.),#3664) ;
#3697 = MEASURE_REPRESENTATION_ITEM('density measure',
POSITIVE_RATIO_MEASURE(7850.),#3665) ;
#3698 = MEASURE_REPRESENTATION_ITEM('density measure',
POSITIVE_RATIO_MEASURE(7850.),#3666) ;
#3699 = MEASURE_REPRESENTATION_ITEM('density measure',
POSITIVE_RATIO_MEASURE(7850.),#3667) ;
#3700 = MEASURE_REPRESENTATION_ITEM('density measure',
POSITIVE_RATIO_MEASURE(7850.),#3668) ;
#3701 = MEASURE_REPRESENTATION_ITEM('density measure',
POSITIVE_RATIO_MEASURE(7850.),#3669) ;
#3702 = MEASURE_REPRESENTATION_ITEM('density measure',
POSITIVE_RATIO_MEASURE(7850.),#3670) ;
#3703 = MEASURE_REPRESENTATION_ITEM('density measure',
POSITIVE_RATIO_MEASURE(7850.),#3671) ;
#3704 = MEASURE_REPRESENTATION_ITEM('density measure',
POSITIVE_RATIO_MEASURE(7850.),#3672) ;
#3705 = MEASURE_REPRESENTATION_ITEM('density measure',
POSITIVE_RATIO_MEASURE(7850.),#3673) ;
#3706 = MEASURE_REPRESENTATION_ITEM('density measure',
POSITIVE_RATIO_MEASURE(7850.),#3674) ;
#3707 = MEASURE_REPRESENTATION_ITEM('density measure',
POSITIVE_RATIO_MEASURE(7850.),#3675) ;
#3708 = MEASURE_REPRESENTATION_ITEM('density measure',
POSITIVE_RATIO_MEASURE(7850.),#3676) ;
#3709 = MEASURE_REPRESENTATION_ITEM('density measure',
POSITIVE_RATIO_MEASURE(7850.),#3677) ;
#3710 = MEASURE_REPRESENTATION_ITEM('density measure',
POSITIVE_RATIO_MEASURE(7850.),#3678) ;
#3711 = MEASURE_REPRESENTATION_ITEM('density measure',
POSITIVE_RATIO_MEASURE(7850.),#3679) ;
#3712 = MEASURE_REPRESENTATION_ITEM('density measure',
POSITIVE_RATIO_MEASURE(7850.),#3680) ;
#3713 = MEASURE_REPRESENTATION_ITEM('density measure',
POSITIVE_RATIO_MEASURE(7850.),#3681) ;
#3714 = MEASURE_REPRESENTATION_ITEM('density measure',
POSITIVE_RATIO_MEASURE(7850.),#3682) ;
#3715 = MEASURE_REPRESENTATION_ITEM('density measure',
POSITIVE_RATIO_MEASURE(7850.),#3683) ;
#3716 = MEASURE_REPRESENTATION_ITEM('density measure',
POSITIVE_RATIO_MEASURE(7850.),#3684) ;
#3717 = MEASURE_REPRESENTATION_ITEM('density measure',
POSITIVE_RATIO_MEASURE(7850.),#3685) ;
#3718 = MEASURE_REPRESENTATION_ITEM('density measure',
POSITIVE_RATIO_MEASURE(7850.),#3686) ;
#3719 = PROPERTY_DEFINITION_REPRESENTATION(#3879,#3783) ;
#3720 = PROPERTY_DEFINITION_REPRESENTATION(#3880,#3784) ;
#3721 = PROPERTY_DEFINITION_REPRESENTATION(#3881,#3785) ;
#3722 = PROPERTY_DEFINITION_REPRESENTATION(#3882,#3786) ;
#3723 = PROPERTY_DEFINITION_REPRESENTATION(#3883,#3787) ;
#3724 = PROPERTY_DEFINITION_REPRESENTATION(#3884,#3788) ;
#3725 = PROPERTY_DEFINITION_REPRESENTATION(#3885,#3789) ;
#3726 = PROPERTY_DEFINITION_REPRESENTATION(#3886,#3790) ;
#3727 = PROPERTY_DEFINITION_REPRESENTATION(#3887,#3791) ;
#3728 = PROPERTY_DEFINITION_REPRESENTATION(#3888,#3792) ;
#3729 = PROPERTY_DEFINITION_REPRESENTATION(#3889,#3793) ;
#3730 = PROPERTY_DEFINITION_REPRESENTATION(#3890,#3794) ;
#3731 = PROPERTY_DEFINITION_REPRESENTATION(#3891,#3795) ;
#3732 = PROPERTY_DEFINITION_REPRESENTATION(#3892,#3796) ;
#3733 = PROPERTY_DEFINITION_REPRESENTATION(#3893,#3797) ;
#3734 = PROPERTY_DEFINITION_REPRESENTATION(#3894,#3798) ;
#3735 = PROPERTY_DEFINITION_REPRESENTATION(#3895,#3799) ;
#3736 = PROPERTY_DEFINITION_REPRESENTATION(#3896,#3800) ;
#3737 = PROPERTY_DEFINITION_REPRESENTATION(#3897,#3801) ;
#3738 = PROPERTY_DEFINITION_REPRESENTATION(#3898,#3802) ;
#3739 = PROPERTY_DEFINITION_REPRESENTATION(#3899,#3803) ;
#3740 = PROPERTY_DEFINITION_REPRESENTATION(#3900,#3804) ;
#3741 = PROPERTY_DEFINITION_REPRESENTATION(#3901,#3805) ;
#3742 = PROPERTY_DEFINITION_REPRESENTATION(#3902,#3806) ;
#3743 = PROPERTY_DEFINITION_REPRESENTATION(#3903,#3807) ;
#3744 = PROPERTY_DEFINITION_REPRESENTATION(#3904,#3808) ;
#3745 = PROPERTY_DEFINITION_REPRESENTATION(#3905,#3809) ;
#3746 = PROPERTY_DEFINITION_REPRESENTATION(#3906,#3810) ;
#3747 = PROPERTY_DEFINITION_REPRESENTATION(#3907,#3811) ;
#3748 = PROPERTY_DEFINITION_REPRESENTATION(#3908,#3812) ;
#3749 = PROPERTY_DEFINITION_REPRESENTATION(#3909,#3813) ;
#3750 = PROPERTY_DEFINITION_REPRESENTATION(#3910,#3814) ;
#3751 = PROPERTY_DEFINITION_REPRESENTATION(#3911,#3815) ;
#3752 = PROPERTY_DEFINITION_REPRESENTATION(#3912,#3816) ;
#3753 = PROPERTY_DEFINITION_REPRESENTATION(#3913,#3817) ;
#3754 = PROPERTY_DEFINITION_REPRESENTATION(#3914,#3818) ;
#3755 = PROPERTY_DEFINITION_REPRESENTATION(#3915,#3819) ;
#3756 = PROPERTY_DEFINITION_REPRESENTATION(#3916,#3820) ;
#3757 = PROPERTY_DEFINITION_REPRESENTATION(#3917,#3821) ;
#3758 = PROPERTY_DEFINITION_REPRESENTATION(#3918,#3822) ;
#3759 = PROPERTY_DEFINITION_REPRESENTATION(#3919,#3823) ;
#3760 = PROPERTY_DEFINITION_REPRESENTATION(#3920,#3824) ;
#3761 = PROPERTY_DEFINITION_REPRESENTATION(#3921,#3825) ;
#3762 = PROPERTY_DEFINITION_REPRESENTATION(#3922,#3826) ;
#3763 = PROPERTY_DEFINITION_REPRESENTATION(#3923,#3827) ;
#3764 = PROPERTY_DEFINITION_REPRESENTATION(#3924,#3828) ;
#3765 = PROPERTY_DEFINITION_REPRESENTATION(#3925,#3829) ;
#3766 = PROPERTY_DEFINITION_REPRESENTATION(#3926,#3830) ;
#3767 = PROPERTY_DEFINITION_REPRESENTATION(#3927,#3831) ;
#3768 = PROPERTY_DEFINITION_REPRESENTATION(#3928,#3832) ;
#3769 = PROPERTY_DEFINITION_REPRESENTATION(#3929,#3833) ;
#3770 = PROPERTY_DEFINITION_REPRESENTATION(#3930,#3834) ;
#3771 = PROPERTY_DEFINITION_REPRESENTATION(#3931,#3835) ;
#3772 = PROPERTY_DEFINITION_REPRESENTATION(#3932,#3836) ;
#3773 = PROPERTY_DEFINITION_REPRESENTATION(#3933,#3837) ;
#3774 = PROPERTY_DEFINITION_REPRESENTATION(#3934,#3838) ;
#3775 = PROPERTY_DEFINITION_REPRESENTATION(#3935,#3839) ;
#3776 = PROPERTY_DEFINITION_REPRESENTATION(#3936,#3840) ;
#3777 = PROPERTY_DEFINITION_REPRESENTATION(#3937,#3841) ;
#3778 = PROPERTY_DEFINITION_REPRESENTATION(#3938,#3842) ;
#3779 = PROPERTY_DEFINITION_REPRESENTATION(#3939,#3843) ;
#3780 = PROPERTY_DEFINITION_REPRESENTATION(#3940,#3844) ;
#3781 = PROPERTY_DEFINITION_REPRESENTATION(#3941,#3845) ;
#3782 = PROPERTY_DEFINITION_REPRESENTATION(#3942,#3846) ;
#3783 = REPRESENTATION('material name',(#3847),#10300) ;
#3784 = REPRESENTATION('density',(#3687),#10300) ;
#3785 = REPRESENTATION('material name',(#3848),#10301) ;
#3786 = REPRESENTATION('density',(#3688),#10301) ;
#3787 = REPRESENTATION('material name',(#3849),#10302) ;
#3788 = REPRESENTATION('density',(#3689),#10302) ;
#3789 = REPRESENTATION('material name',(#3850),#10303) ;
#3790 = REPRESENTATION('density',(#3690),#10303) ;
#3791 = REPRESENTATION('material name',(#3851),#10304) ;
#3792 = REPRESENTATION('density',(#3691),#10304) ;
#3793 = REPRESENTATION('material name',(#3852),#10305) ;
#3794 = REPRESENTATION('density',(#3692),#10305) ;
#3795 = REPRESENTATION('material name',(#3853),#10306) ;
#3796 = REPRESENTATION('density',(#3693),#10306) ;
#3797 = REPRESENTATION('material name',(#3854),#10307) ;
#3798 = REPRESENTATION('density',(#3694),#10307) ;
#3799 = REPRESENTATION('material name',(#3855),#10308) ;
#3800 = REPRESENTATION('density',(#3695),#10308) ;
#3801 = REPRESENTATION('material name',(#3856),#10309) ;
#3802 = REPRESENTATION('density',(#3696),#10309) ;
#3803 = REPRESENTATION('material name',(#3857),#10310) ;
#3804 = REPRESENTATION('density',(#3697),#10310) ;
#3805 = REPRESENTATION('material name',(#3858),#10311) ;
#3806 = REPRESENTATION('density',(#3698),#10311) ;
#3807 = REPRESENTATION('material name',(#3859),#10312) ;
#3808 = REPRESENTATION('density',(#3699),#10312) ;
#3809 = REPRESENTATION('material name',(#3860),#10313) ;
#3810 = REPRESENTATION('density',(#3700),#10313) ;
#3811 = REPRESENTATION('material name',(#3861),#10314) ;
#3812 = REPRESENTATION('density',(#3701),#10314) ;
#3813 = REPRESENTATION('material name',(#3862),#10315) ;
#3814 = REPRESENTATION('density',(#3702),#10315) ;
#3815 = REPRESENTATION('material name',(#3863),#10316) ;
#3816 = REPRESENTATION('density',(#3703),#10316) ;
#3817 = REPRESENTATION('material name',(#3864),#10317) ;
#3818 = REPRESENTATION('density',(#3704),#10317) ;
#3819 = REPRESENTATION('material name',(#3865),#10318) ;
#3820 = REPRESENTATION('density',(#3705),#10318) ;
#3821 = REPRESENTATION('material name',(#3866),#10319) ;
#3822 = REPRESENTATION('density',(#3706),#10319) ;
#3823 = REPRESENTATION('material name',(#3867),#10320) ;
#3824 = REPRESENTATION('density',(#3707),#10320) ;
#3825 = REPRESENTATION('material name',(#3868),#10321) ;
#3826 = REPRESENTATION('density',(#3708),#10321) ;
#3827 = REPRESENTATION('material name',(#3869),#10322) ;
#3828 = REPRESENTATION('density',(#3709),#10322) ;
#3829 = REPRESENTATION('material name',(#3870),#10323) ;
#3830 = REPRESENTATION('density',(#3710),#10323) ;
#3831 = REPRESENTATION('material name',(#3871),#10325) ;
#3832 = REPRESENTATION('density',(#3711),#10325) ;
#3833 = REPRESENTATION('material name',(#3872),#10326) ;
#3834 = REPRESENTATION('density',(#3712),#10326) ;
#3835 = REPRESENTATION('material name',(#3873),#10327) ;
#3836 = REPRESENTATION('density',(#3713),#10327) ;
#3837 = REPRESENTATION('material name',(#3874),#10329) ;
#3838 = REPRESENTATION('density',(#3714),#10329) ;
#3839 = REPRESENTATION('material name',(#3875),#10330) ;
#3840 = REPRESENTATION('density',(#3715),#10330) ;
#3841 = REPRESENTATION('material name',(#3876),#10331) ;
#3842 = REPRESENTATION('density',(#3716),#10331) ;
#3843 = REPRESENTATION('material name',(#3877),#10332) ;
#3844 = REPRESENTATION('density',(#3717),#10332) ;
#3845 = REPRESENTATION('material name',(#3878),#10333) ;
#3846 = REPRESENTATION('density',(#3718),#10333) ;
#3847 = DESCRIPTIVE_REPRESENTATION_ITEM('Steel','Steel') ;
#3848 = DESCRIPTIVE_REPRESENTATION_ITEM('Steel','Steel') ;
#3849 = DESCRIPTIVE_REPRESENTATION_ITEM('Steel','Steel') ;
#3850 = DESCRIPTIVE_REPRESENTATION_ITEM('Steel','Steel') ;
#3851 = DESCRIPTIVE_REPRESENTATION_ITEM('Steel','Steel') ;
#3852 = DESCRIPTIVE_REPRESENTATION_ITEM('Steel','Steel') ;
#3853 = DESCRIPTIVE_REPRESENTATION_ITEM('Steel','Steel') ;
#3854 = DESCRIPTIVE_REPRESENTATION_ITEM('Steel','Steel') ;
#3855 = DESCRIPTIVE_REPRESENTATION_ITEM('Steel','Steel') ;
#3856 = DESCRIPTIVE_REPRESENTATION_ITEM('Steel','Steel') ;
#3857 = DESCRIPTIVE_REPRESENTATION_ITEM('Steel','Steel') ;
#3858 = DESCRIPTIVE_REPRESENTATION_ITEM('Steel','Steel') ;
#3859 = DESCRIPTIVE_REPRESENTATION_ITEM('Steel','Steel') ;
#3860 = DESCRIPTIVE_REPRESENTATION_ITEM('Steel','Steel') ;
#3861 = DESCRIPTIVE_REPRESENTATION_ITEM('Steel','Steel') ;
#3862 = DESCRIPTIVE_REPRESENTATION_ITEM('Steel','Steel') ;
#3863 = DESCRIPTIVE_REPRESENTATION_ITEM('Steel','Steel') ;
#3864 = DESCRIPTIVE_REPRESENTATION_ITEM('Steel','Steel') ;
#3865 = DESCRIPTIVE_REPRESENTATION_ITEM('Steel','Steel') ;
#3866 = DESCRIPTIVE_REPRESENTATION_ITEM('Steel','Steel') ;
#3867 = DESCRIPTIVE_REPRESENTATION_ITEM('Steel','Steel') ;
#3868 = DESCRIPTIVE_REPRESENTATION_ITEM('Steel','Steel') ;
#3869 = DESCRIPTIVE_REPRESENTATION_ITEM('Steel','Steel') ;
#3870 = DESCRIPTIVE_REPRESENTATION_ITEM('Steel','Steel') ;
#3871 = DESCRIPTIVE_REPRESENTATION_ITEM('Steel','Steel') ;
#3872 = DESCRIPTIVE_REPRESENTATION_ITEM('Steel','Steel') ;
#3873 = DESCRIPTIVE_REPRESENTATION_ITEM('Steel','Steel') ;
#3874 = DESCRIPTIVE_REPRESENTATION_ITEM('Steel','Steel') ;
#3875 = DESCRIPTIVE_REPRESENTATION_ITEM('Steel','Steel') ;
#3876 = DESCRIPTIVE_REPRESENTATION_ITEM('Steel','Steel') ;
#3877 = DESCRIPTIVE_REPRESENTATION_ITEM('Steel','Steel') ;
#3878 = DESCRIPTIVE_REPRESENTATION_ITEM('Steel','Steel') ;
#3879 = PROPERTY_DEFINITION('material property','material name',#10485) ;
#3880 = PROPERTY_DEFINITION('material property','density of part',#10485) ;
#3881 = PROPERTY_DEFINITION('material property','material name',#10486) ;
#3882 = PROPERTY_DEFINITION('material property','density of part',#10486) ;
#3883 = PROPERTY_DEFINITION('material property','material name',#10487) ;
#3884 = PROPERTY_DEFINITION('material property','density of part',#10487) ;
#3885 = PROPERTY_DEFINITION('material property','material name',#10488) ;
#3886 = PROPERTY_DEFINITION('material property','density of part',#10488) ;
#3887 = PROPERTY_DEFINITION('material property','material name',#10489) ;
#3888 = PROPERTY_DEFINITION('material property','density of part',#10489) ;
#3889 = PROPERTY_DEFINITION('material property','material name',#10490) ;
#3890 = PROPERTY_DEFINITION('material property','density of part',#10490) ;
#3891 = PROPERTY_DEFINITION('material property','material name',#10491) ;
#3892 = PROPERTY_DEFINITION('material property','density of part',#10491) ;
#3893 = PROPERTY_DEFINITION('material property','material name',#10492) ;
#3894 = PROPERTY_DEFINITION('material property','density of part',#10492) ;
#3895 = PROPERTY_DEFINITION('material property','material name',#10493) ;
#3896 = PROPERTY_DEFINITION('material property','density of part',#10493) ;
#3897 = PROPERTY_DEFINITION('material property','material name',#10494) ;
#3898 = PROPERTY_DEFINITION('material property','density of part',#10494) ;
#3899 = PROPERTY_DEFINITION('material property','material name',#10495) ;
#3900 = PROPERTY_DEFINITION('material property','density of part',#10495) ;
#3901 = PROPERTY_DEFINITION('material property','material name',#10496) ;
#3902 = PROPERTY_DEFINITION('material property','density of part',#10496) ;
#3903 = PROPERTY_DEFINITION('material property','material name',#10497) ;
#3904 = PROPERTY_DEFINITION('material property','density of part',#10497) ;
#3905 = PROPERTY_DEFINITION('material property','material name',#10498) ;
#3906 = PROPERTY_DEFINITION('material property','density of part',#10498) ;
#3907 = PROPERTY_DEFINITION('material property','material name',#10499) ;
#3908 = PROPERTY_DEFINITION('material property','density of part',#10499) ;
#3909 = PROPERTY_DEFINITION('material property','material name',#10500) ;
#3910 = PROPERTY_DEFINITION('material property','density of part',#10500) ;
#3911 = PROPERTY_DEFINITION('material property','material name',#10501) ;
#3912 = PROPERTY_DEFINITION('material property','density of part',#10501) ;
#3913 = PROPERTY_DEFINITION('material property','material name',#10502) ;
#3914 = PROPERTY_DEFINITION('material property','density of part',#10502) ;
#3915 = PROPERTY_DEFINITION('material property','material name',#10503) ;
#3916 = PROPERTY_DEFINITION('material property','density of part',#10503) ;
#3917 = PROPERTY_DEFINITION('material property','material name',#10504) ;
#3918 = PROPERTY_DEFINITION('material property','density of part',#10504) ;
#3919 = PROPERTY_DEFINITION('material property','material name',#10505) ;
#3920 = PROPERTY_DEFINITION('material property','density of part',#10505) ;
#3921 = PROPERTY_DEFINITION('material property','material name',#10506) ;
#3922 = PROPERTY_DEFINITION('material property','density of part',#10506) ;
#3923 = PROPERTY_DEFINITION('material property','material name',#10507) ;
#3924 = PROPERTY_DEFINITION('material property','density of part',#10507) ;
#3925 = PROPERTY_DEFINITION('material property','material name',#10508) ;
#3926 = PROPERTY_DEFINITION('material property','density of part',#10508) ;
#3927 = PROPERTY_DEFINITION('material property','material name',#10510) ;
#3928 = PROPERTY_DEFINITION('material property','density of part',#10510) ;
#3929 = PROPERTY_DEFINITION('material property','material name',#10511) ;
#3930 = PROPERTY_DEFINITION('material property','density of part',#10511) ;
#3931 = PROPERTY_DEFINITION('material property','material name',#10512) ;
#3932 = PROPERTY_DEFINITION('material property','density of part',#10512) ;
#3933 = PROPERTY_DEFINITION('material property','material name',#10514) ;
#3934 = PROPERTY_DEFINITION('material property','density of part',#10514) ;
#3935 = PROPERTY_DEFINITION('material property','material name',#10515) ;
#3936 = PROPERTY_DEFINITION('material property','density of part',#10515) ;
#3937 = PROPERTY_DEFINITION('material property','material name',#10516) ;
#3938 = PROPERTY_DEFINITION('material property','density of part',#10516) ;
#3939 = PROPERTY_DEFINITION('material property','material name',#10517) ;
#3940 = PROPERTY_DEFINITION('material property','density of part',#10517) ;
#3941 = PROPERTY_DEFINITION('material property','material name',#10518) ;
#3942 = PROPERTY_DEFINITION('material property','density of part',#10518) ;
#3943 = AXIS2_PLACEMENT_3D('',#5604,#4444,#4445) ;
#3944 = AXIS2_PLACEMENT_3D('',#5605,#4446,#4447) ;
#3945 = AXIS2_PLACEMENT_3D('',#5606,#4448,#4449) ;
#3946 = AXIS2_PLACEMENT_3D('',#5607,#4450,#4451) ;
#3947 = AXIS2_PLACEMENT_3D('',#5610,#4452,#4453) ;
#3948 = AXIS2_PLACEMENT_3D('',#5611,#4454,#4455) ;
#3949 = AXIS2_PLACEMENT_3D('',#5613,#4456,#4457) ;
#3950 = AXIS2_PLACEMENT_3D('',#5614,#4458,#4459) ;
#3951 = AXIS2_PLACEMENT_3D('',#5615,#4460,#4461) ;
#3952 = AXIS2_PLACEMENT_3D('',#5617,#4462,#4463) ;
#3953 = AXIS2_PLACEMENT_3D('',#5619,#4464,#4465) ;
#3954 = AXIS2_PLACEMENT_3D('',#5621,#4466,#4467) ;
#3955 = AXIS2_PLACEMENT_3D('',#5622,#4468,#4469) ;
#3956 = AXIS2_PLACEMENT_3D('',#5623,#4470,#4471) ;
#3957 = AXIS2_PLACEMENT_3D('',#5625,#4473,#4474) ;
#3958 = AXIS2_PLACEMENT_3D('',#5626,#4475,#4476) ;
#3959 = AXIS2_PLACEMENT_3D('',#5627,#4477,#4478) ;
#3960 = AXIS2_PLACEMENT_3D('',#5630,#4479,#4480) ;
#3961 = AXIS2_PLACEMENT_3D('',#5631,#4481,#4482) ;
#3962 = AXIS2_PLACEMENT_3D('',#5633,#4483,#4484) ;
#3963 = AXIS2_PLACEMENT_3D('',#5635,#4485,#4486) ;
#3964 = AXIS2_PLACEMENT_3D('',#5636,#4487,#4488) ;
#3965 = AXIS2_PLACEMENT_3D('',#5637,#4489,#4490) ;
#3966 = AXIS2_PLACEMENT_3D('',#5641,#4492,#4493) ;
#3967 = AXIS2_PLACEMENT_3D('',#5642,#4494,#4495) ;
#3968 = AXIS2_PLACEMENT_3D('',#5643,#4496,#4497) ;
#3969 = AXIS2_PLACEMENT_3D('',#5646,#4498,#4499) ;
#3970 = AXIS2_PLACEMENT_3D('',#5647,#4500,#4501) ;
#3971 = AXIS2_PLACEMENT_3D('',#5648,#4502,#4503) ;
#3972 = AXIS2_PLACEMENT_3D('',#5649,#4504,#4505) ;
#3973 = AXIS2_PLACEMENT_3D('',#5651,#4507,#4508) ;
#3974 = AXIS2_PLACEMENT_3D('',#5652,#4509,#4510) ;
#3975 = AXIS2_PLACEMENT_3D('',#5654,#4511,#4512) ;
#3976 = AXIS2_PLACEMENT_3D('',#5655,#4513,#4514) ;
#3977 = AXIS2_PLACEMENT_3D('',#5656,#4515,#4516) ;
#3978 = AXIS2_PLACEMENT_3D('',#5657,#4517,#4518) ;
#3979 = AXIS2_PLACEMENT_3D('',#5659,#4519,#4520) ;
#3980 = AXIS2_PLACEMENT_3D('',#5660,#4521,#4522) ;
#3981 = AXIS2_PLACEMENT_3D('',#5661,#4523,#4524) ;
#3982 = AXIS2_PLACEMENT_3D('',#5662,#4525,#4526) ;
#3983 = AXIS2_PLACEMENT_3D('',#5664,#4527,#4528) ;
#3984 = AXIS2_PLACEMENT_3D('',#5665,#4529,#4530) ;
#3985 = AXIS2_PLACEMENT_3D('',#5666,#4531,#4532) ;
#3986 = AXIS2_PLACEMENT_3D('',#5667,#4533,#4534) ;
#3987 = AXIS2_PLACEMENT_3D('',#5669,#4535,#4536) ;
#3988 = AXIS2_PLACEMENT_3D('',#5670,#4537,#4538) ;
#3989 = AXIS2_PLACEMENT_3D('',#5671,#4539,#4540) ;
#3990 = AXIS2_PLACEMENT_3D('',#5672,#4541,#4542) ;
#3991 = AXIS2_PLACEMENT_3D('',#5674,#4543,#4544) ;
#3992 = AXIS2_PLACEMENT_3D('',#5675,#4545,#4546) ;
#3993 = AXIS2_PLACEMENT_3D('',#5676,#4547,#4548) ;
#3994 = AXIS2_PLACEMENT_3D('',#5677,#4549,#4550) ;
#3995 = AXIS2_PLACEMENT_3D('',#5679,#4551,#4552) ;
#3996 = AXIS2_PLACEMENT_3D('',#5680,#4553,#4554) ;
#3997 = AXIS2_PLACEMENT_3D('',#5681,#4555,#4556) ;
#3998 = AXIS2_PLACEMENT_3D('',#5682,#4557,#4558) ;
#3999 = AXIS2_PLACEMENT_3D('',#5684,#4559,#4560) ;
#4000 = AXIS2_PLACEMENT_3D('',#5685,#4561,#4562) ;
#4001 = AXIS2_PLACEMENT_3D('',#5686,#4563,#4564) ;
#4002 = AXIS2_PLACEMENT_3D('',#5687,#4565,#4566) ;
#4003 = AXIS2_PLACEMENT_3D('',#5689,#4567,#4568) ;
#4004 = AXIS2_PLACEMENT_3D('',#5690,#4569,#4570) ;
#4005 = AXIS2_PLACEMENT_3D('',#5691,#4571,#4572) ;
#4006 = AXIS2_PLACEMENT_3D('',#5692,#4573,#4574) ;
#4007 = AXIS2_PLACEMENT_3D('',#5694,#4575,#4576) ;
#4008 = AXIS2_PLACEMENT_3D('',#5695,#4577,#4578) ;
#4009 = AXIS2_PLACEMENT_3D('',#5696,#4579,#4580) ;
#4010 = AXIS2_PLACEMENT_3D('',#5697,#4581,#4582) ;
#4011 = AXIS2_PLACEMENT_3D('',#5699,#4583,#4584) ;
#4012 = AXIS2_PLACEMENT_3D('',#5700,#4585,#4586) ;
#4013 = AXIS2_PLACEMENT_3D('',#5701,#4587,#4588) ;
#4014 = AXIS2_PLACEMENT_3D('',#5702,#4589,#4590) ;
#4015 = AXIS2_PLACEMENT_3D('',#5704,#4591,#4592) ;
#4016 = AXIS2_PLACEMENT_3D('',#5705,#4593,#4594) ;
#4017 = AXIS2_PLACEMENT_3D('',#5706,#4595,#4596) ;
#4018 = AXIS2_PLACEMENT_3D('',#5707,#4597,#4598) ;
#4019 = AXIS2_PLACEMENT_3D('',#5709,#4599,#4600) ;
#4020 = AXIS2_PLACEMENT_3D('',#5710,#4601,#4602) ;
#4021 = AXIS2_PLACEMENT_3D('',#5711,#4603,#4604) ;
#4022 = AXIS2_PLACEMENT_3D('',#5712,#4605,#4606) ;
#4023 = AXIS2_PLACEMENT_3D('',#5714,#4607,#4608) ;
#4024 = AXIS2_PLACEMENT_3D('',#5715,#4609,#4610) ;
#4025 = AXIS2_PLACEMENT_3D('',#5716,#4611,#4612) ;
#4026 = AXIS2_PLACEMENT_3D('',#5717,#4613,#4614) ;
#4027 = AXIS2_PLACEMENT_3D('',#5719,#4615,#4616) ;
#4028 = AXIS2_PLACEMENT_3D('',#5720,#4617,#4618) ;
#4029 = AXIS2_PLACEMENT_3D('',#5721,#4619,#4620) ;
#4030 = AXIS2_PLACEMENT_3D('',#5722,#4621,#4622) ;
#4031 = AXIS2_PLACEMENT_3D('',#5724,#4623,#4624) ;
#4032 = AXIS2_PLACEMENT_3D('',#5725,#4625,#4626) ;
#4033 = AXIS2_PLACEMENT_3D('',#5726,#4627,#4628) ;
#4034 = AXIS2_PLACEMENT_3D('',#5727,#4629,#4630) ;
#4035 = AXIS2_PLACEMENT_3D('',#5729,#4631,#4632) ;
#4036 = AXIS2_PLACEMENT_3D('',#5730,#4633,#4634) ;
#4037 = AXIS2_PLACEMENT_3D('',#5731,#4635,#4636) ;
#4038 = AXIS2_PLACEMENT_3D('',#5732,#4637,#4638) ;
#4039 = AXIS2_PLACEMENT_3D('',#5734,#4639,#4640) ;
#4040 = AXIS2_PLACEMENT_3D('',#5735,#4641,#4642) ;
#4041 = AXIS2_PLACEMENT_3D('',#5736,#4643,#4644) ;
#4042 = AXIS2_PLACEMENT_3D('',#5737,#4645,#4646) ;
#4043 = AXIS2_PLACEMENT_3D('',#5739,#4647,#4648) ;
#4044 = AXIS2_PLACEMENT_3D('',#5740,#4649,#4650) ;
#4045 = AXIS2_PLACEMENT_3D('',#5741,#4651,#4652) ;
#4046 = AXIS2_PLACEMENT_3D('',#5742,#4653,#4654) ;
#4047 = AXIS2_PLACEMENT_3D('',#5744,#4655,#4656) ;
#4048 = AXIS2_PLACEMENT_3D('',#5745,#4657,#4658) ;
#4049 = AXIS2_PLACEMENT_3D('',#5746,#4659,#4660) ;
#4050 = AXIS2_PLACEMENT_3D('',#5747,#4661,#4662) ;
#4051 = AXIS2_PLACEMENT_3D('',#5749,#4663,#4664) ;
#4052 = AXIS2_PLACEMENT_3D('',#5750,#4665,#4666) ;
#4053 = AXIS2_PLACEMENT_3D('',#5751,#4667,#4668) ;
#4054 = AXIS2_PLACEMENT_3D('',#5752,#4669,#4670) ;
#4055 = AXIS2_PLACEMENT_3D('',#5754,#4671,#4672) ;
#4056 = AXIS2_PLACEMENT_3D('',#5755,#4673,#4674) ;
#4057 = AXIS2_PLACEMENT_3D('',#5756,#4675,#4676) ;
#4058 = AXIS2_PLACEMENT_3D('',#5757,#4677,#4678) ;
#4059 = AXIS2_PLACEMENT_3D('',#5759,#4679,#4680) ;
#4060 = AXIS2_PLACEMENT_3D('',#5760,#4681,#4682) ;
#4061 = AXIS2_PLACEMENT_3D('',#5761,#4683,#4684) ;
#4062 = AXIS2_PLACEMENT_3D('',#5762,#4685,#4686) ;
#4063 = AXIS2_PLACEMENT_3D('',#5763,#4687,#4688) ;
#4064 = AXIS2_PLACEMENT_3D('',#5764,#4689,#4690) ;
#4065 = AXIS2_PLACEMENT_3D('',#5765,#4691,#4692) ;
#4066 = AXIS2_PLACEMENT_3D('',#5766,#4693,#4694) ;
#4067 = AXIS2_PLACEMENT_3D('',#5767,#4695,#4696) ;
#4068 = AXIS2_PLACEMENT_3D('',#5768,#4697,#4698) ;
#4069 = AXIS2_PLACEMENT_3D('',#5769,#4699,#4700) ;
#4070 = AXIS2_PLACEMENT_3D('',#5770,#4701,#4702) ;
#4071 = AXIS2_PLACEMENT_3D('',#5771,#4703,#4704) ;
#4072 = AXIS2_PLACEMENT_3D('',#5772,#4705,#4706) ;
#4073 = AXIS2_PLACEMENT_3D('',#5773,#4707,#4708) ;
#4074 = AXIS2_PLACEMENT_3D('',#5774,#4709,#4710) ;
#4075 = AXIS2_PLACEMENT_3D('',#5775,#4711,#4712) ;
#4076 = AXIS2_PLACEMENT_3D('',#5776,#4713,#4714) ;
#4077 = AXIS2_PLACEMENT_3D('',#5777,#4715,#4716) ;
#4078 = AXIS2_PLACEMENT_3D('',#5778,#4717,#4718) ;
#4079 = AXIS2_PLACEMENT_3D('',#5779,#4719,#4720) ;
#4080 = AXIS2_PLACEMENT_3D('',#5780,#4721,#4722) ;
#4081 = AXIS2_PLACEMENT_3D('',#5781,#4723,#4724) ;
#4082 = AXIS2_PLACEMENT_3D('',#5782,#4725,#4726) ;
#4083 = AXIS2_PLACEMENT_3D('',#5783,#4727,#4728) ;
#4084 = AXIS2_PLACEMENT_3D('',#5784,#4729,#4730) ;
#4085 = AXIS2_PLACEMENT_3D('',#5785,#4731,#4732) ;
#4086 = AXIS2_PLACEMENT_3D('',#5786,#4733,#4734) ;
#4087 = AXIS2_PLACEMENT_3D('',#5787,#4735,#4736) ;
#4088 = AXIS2_PLACEMENT_3D('',#5789,#4737,#4738) ;
#4089 = AXIS2_PLACEMENT_3D('',#5798,#4740,#4741) ;
#4090 = AXIS2_PLACEMENT_3D('',#5801,#4743,#4744) ;
#4091 = AXIS2_PLACEMENT_3D('',#5803,#4745,#4746) ;
#4092 = AXIS2_PLACEMENT_3D('',#6041,#4749,#4750) ;
#4093 = AXIS2_PLACEMENT_3D('',#6209,#4752,#4753) ;
#4094 = AXIS2_PLACEMENT_3D('',#6340,#4755,#4756) ;
#4095 = AXIS2_PLACEMENT_3D('',#6470,#4758,#4759) ;
#4096 = AXIS2_PLACEMENT_3D('',#6471,#4760,#4761) ;
#4097 = AXIS2_PLACEMENT_3D('',#6502,#4764,#4765) ;
#4098 = AXIS2_PLACEMENT_3D('',#6659,#4766,#4767) ;
#4099 = AXIS2_PLACEMENT_3D('',#6677,#4768,#4769) ;
#4100 = AXIS2_PLACEMENT_3D('',#6871,#4770,#4771) ;
#4101 = AXIS2_PLACEMENT_3D('',#6873,#4773,#4774) ;
#4102 = AXIS2_PLACEMENT_3D('',#6875,#4776,#4777) ;
#4103 = AXIS2_PLACEMENT_3D('',#6877,#4779,#4780) ;
#4104 = AXIS2_PLACEMENT_3D('',#6904,#4781,#4782) ;
#4105 = AXIS2_PLACEMENT_3D('',#7109,#4783,#4784) ;
#4106 = AXIS2_PLACEMENT_3D('',#7140,#4787,#4788) ;
#4107 = AXIS2_PLACEMENT_3D('',#7297,#4789,#4790) ;
#4108 = AXIS2_PLACEMENT_3D('',#7315,#4791,#4792) ;
#4109 = AXIS2_PLACEMENT_3D('',#7509,#4793,#4794) ;
#4110 = AXIS2_PLACEMENT_3D('',#7511,#4796,#4797) ;
#4111 = AXIS2_PLACEMENT_3D('',#7513,#4799,#4800) ;
#4112 = AXIS2_PLACEMENT_3D('',#7515,#4802,#4803) ;
#4113 = AXIS2_PLACEMENT_3D('',#7746,#4804,#4805) ;
#4114 = AXIS2_PLACEMENT_3D('',#7747,#4806,#4807) ;
#4115 = AXIS2_PLACEMENT_3D('',#7778,#4810,#4811) ;
#4116 = AXIS2_PLACEMENT_3D('',#7935,#4812,#4813) ;
#4117 = AXIS2_PLACEMENT_3D('',#7953,#4814,#4815) ;
#4118 = AXIS2_PLACEMENT_3D('',#8147,#4816,#4817) ;
#4119 = AXIS2_PLACEMENT_3D('',#8149,#4819,#4820) ;
#4120 = AXIS2_PLACEMENT_3D('',#8151,#4822,#4823) ;
#4121 = AXIS2_PLACEMENT_3D('',#8153,#4825,#4826) ;
#4122 = AXIS2_PLACEMENT_3D('',#8384,#4827,#4828) ;
#4123 = AXIS2_PLACEMENT_3D('',#8415,#4831,#4832) ;
#4124 = AXIS2_PLACEMENT_3D('',#8572,#4833,#4834) ;
#4125 = AXIS2_PLACEMENT_3D('',#8590,#4835,#4836) ;
#4126 = AXIS2_PLACEMENT_3D('',#8784,#4837,#4838) ;
#4127 = AXIS2_PLACEMENT_3D('',#8786,#4840,#4841) ;
#4128 = AXIS2_PLACEMENT_3D('',#8788,#4843,#4844) ;
#4129 = AXIS2_PLACEMENT_3D('',#8790,#4846,#4847) ;
#4130 = AXIS2_PLACEMENT_3D('',#9021,#4848,#4849) ;
#4131 = AXIS2_PLACEMENT_3D('',#9052,#4852,#4853) ;
#4132 = AXIS2_PLACEMENT_3D('',#9209,#4854,#4855) ;
#4133 = AXIS2_PLACEMENT_3D('',#9227,#4856,#4857) ;
#4134 = AXIS2_PLACEMENT_3D('',#9421,#4858,#4859) ;
#4135 = AXIS2_PLACEMENT_3D('',#9423,#4861,#4862) ;
#4136 = AXIS2_PLACEMENT_3D('',#9425,#4864,#4865) ;
#4137 = AXIS2_PLACEMENT_3D('',#9427,#4867,#4868) ;
#4138 = AXIS2_PLACEMENT_3D('',#9658,#4869,#4870) ;
#4139 = AXIS2_PLACEMENT_3D('',#9659,#4871,#4872) ;
#4140 = AXIS2_PLACEMENT_3D('',#9661,#4873,#4874) ;
#4141 = AXIS2_PLACEMENT_3D('',#9664,#4876,#4877) ;
#4142 = AXIS2_PLACEMENT_3D('',#9665,#4878,#4879) ;
#4143 = AXIS2_PLACEMENT_3D('',#9667,#4880,#4881) ;
#4144 = AXIS2_PLACEMENT_3D('',#9670,#4883,#4884) ;
#4145 = AXIS2_PLACEMENT_3D('',#9671,#4885,#4886) ;
#4146 = AXIS2_PLACEMENT_3D('',#9672,#4887,#4888) ;
#4147 = AXIS2_PLACEMENT_3D('',#9673,#4889,#4890) ;
#4148 = AXIS2_PLACEMENT_3D('',#9674,#4891,#4892) ;
#4149 = AXIS2_PLACEMENT_3D('',#9683,#4897,#4898) ;
#4150 = AXIS2_PLACEMENT_3D('',#9692,#4903,#4904) ;
#4151 = AXIS2_PLACEMENT_3D('',#9701,#4909,#4910) ;
#4152 = AXIS2_PLACEMENT_3D('',#9710,#4915,#4916) ;
#4153 = AXIS2_PLACEMENT_3D('',#9711,#4917,#4918) ;
#4154 = AXIS2_PLACEMENT_3D('',#9712,#4919,#4920) ;
#4155 = AXIS2_PLACEMENT_3D('',#9713,#4921,#4922) ;
#4156 = AXIS2_PLACEMENT_3D('',#9714,#4923,#4924) ;
#4157 = AXIS2_PLACEMENT_3D('',#9715,#4925,#4926) ;
#4158 = AXIS2_PLACEMENT_3D('',#9716,#4927,#4928) ;
#4159 = AXIS2_PLACEMENT_3D('',#9717,#4929,#4930) ;
#4160 = AXIS2_PLACEMENT_3D('',#9718,#4931,#4932) ;
#4161 = AXIS2_PLACEMENT_3D('',#9719,#4933,#4934) ;
#4162 = AXIS2_PLACEMENT_3D('',#9720,#4935,#4936) ;
#4163 = AXIS2_PLACEMENT_3D('',#9721,#4937,#4938) ;
#4164 = AXIS2_PLACEMENT_3D('',#9722,#4939,#4940) ;
#4165 = AXIS2_PLACEMENT_3D('',#9723,#4941,#4942) ;
#4166 = AXIS2_PLACEMENT_3D('',#9724,#4943,#4944) ;
#4167 = AXIS2_PLACEMENT_3D('',#9725,#4945,#4946) ;
#4168 = AXIS2_PLACEMENT_3D('',#9726,#4947,#4948) ;
#4169 = AXIS2_PLACEMENT_3D('',#9727,#4949,#4950) ;
#4170 = AXIS2_PLACEMENT_3D('',#9728,#4951,#4952) ;
#4171 = AXIS2_PLACEMENT_3D('',#9729,#4953,#4954) ;
#4172 = AXIS2_PLACEMENT_3D('',#9731,#4955,#4956) ;
#4173 = AXIS2_PLACEMENT_3D('',#9734,#4958,#4959) ;
#4174 = AXIS2_PLACEMENT_3D('',#9735,#4960,#4961) ;
#4175 = AXIS2_PLACEMENT_3D('',#9752,#4970,#4971) ;
#4176 = AXIS2_PLACEMENT_3D('',#9769,#4980,#4981) ;
#4177 = AXIS2_PLACEMENT_3D('',#9772,#4984,#4985) ;
#4178 = AXIS2_PLACEMENT_3D('',#9775,#4988,#4989) ;
#4179 = AXIS2_PLACEMENT_3D('',#9778,#4992,#4993) ;
#4180 = AXIS2_PLACEMENT_3D('',#9781,#4996,#4997) ;
#4181 = AXIS2_PLACEMENT_3D('',#9785,#4999,#5000) ;
#4182 = AXIS2_PLACEMENT_3D('',#9786,#5001,#5002) ;
#4183 = AXIS2_PLACEMENT_3D('',#9787,#5003,#5004) ;
#4184 = AXIS2_PLACEMENT_3D('',#9789,#5005,#5006) ;
#4185 = AXIS2_PLACEMENT_3D('',#9792,#5008,#5009) ;
#4186 = AXIS2_PLACEMENT_3D('',#9793,#5010,#5011) ;
#4187 = AXIS2_PLACEMENT_3D('',#9795,#5013,#5014) ;
#4188 = AXIS2_PLACEMENT_3D('',#9797,#5016,#5017) ;
#4189 = AXIS2_PLACEMENT_3D('',#9803,#5021,#5022) ;
#4190 = AXIS2_PLACEMENT_3D('',#9809,#5026,#5027) ;
#4191 = AXIS2_PLACEMENT_3D('',#9811,#5029,#5030) ;
#4192 = AXIS2_PLACEMENT_3D('',#9813,#5032,#5033) ;
#4193 = AXIS2_PLACEMENT_3D('',#9814,#5034,#5035) ;
#4194 = AXIS2_PLACEMENT_3D('',#9818,#5037,#5038) ;
#4195 = AXIS2_PLACEMENT_3D('',#9819,#5039,#5040) ;
#4196 = AXIS2_PLACEMENT_3D('',#9820,#5041,#5042) ;
#4197 = AXIS2_PLACEMENT_3D('',#9822,#5043,#5044) ;
#4198 = AXIS2_PLACEMENT_3D('',#9825,#5046,#5047) ;
#4199 = AXIS2_PLACEMENT_3D('',#9826,#5048,#5049) ;
#4200 = AXIS2_PLACEMENT_3D('',#9828,#5051,#5052) ;
#4201 = AXIS2_PLACEMENT_3D('',#9830,#5054,#5055) ;
#4202 = AXIS2_PLACEMENT_3D('',#9836,#5059,#5060) ;
#4203 = AXIS2_PLACEMENT_3D('',#9842,#5064,#5065) ;
#4204 = AXIS2_PLACEMENT_3D('',#9844,#5067,#5068) ;
#4205 = AXIS2_PLACEMENT_3D('',#9846,#5070,#5071) ;
#4206 = AXIS2_PLACEMENT_3D('',#9847,#5072,#5073) ;
#4207 = AXIS2_PLACEMENT_3D('',#9851,#5075,#5076) ;
#4208 = AXIS2_PLACEMENT_3D('',#9852,#5077,#5078) ;
#4209 = AXIS2_PLACEMENT_3D('',#9853,#5079,#5080) ;
#4210 = AXIS2_PLACEMENT_3D('',#9855,#5081,#5082) ;
#4211 = AXIS2_PLACEMENT_3D('',#9858,#5084,#5085) ;
#4212 = AXIS2_PLACEMENT_3D('',#9859,#5086,#5087) ;
#4213 = AXIS2_PLACEMENT_3D('',#9861,#5089,#5090) ;
#4214 = AXIS2_PLACEMENT_3D('',#9863,#5092,#5093) ;
#4215 = AXIS2_PLACEMENT_3D('',#9869,#5097,#5098) ;
#4216 = AXIS2_PLACEMENT_3D('',#9875,#5102,#5103) ;
#4217 = AXIS2_PLACEMENT_3D('',#9877,#5105,#5106) ;
#4218 = AXIS2_PLACEMENT_3D('',#9879,#5108,#5109) ;
#4219 = AXIS2_PLACEMENT_3D('',#9880,#5110,#5111) ;
#4220 = AXIS2_PLACEMENT_3D('',#9884,#5113,#5114) ;
#4221 = AXIS2_PLACEMENT_3D('',#9885,#5115,#5116) ;
#4222 = AXIS2_PLACEMENT_3D('',#9886,#5117,#5118) ;
#4223 = AXIS2_PLACEMENT_3D('',#9888,#5119,#5120) ;
#4224 = AXIS2_PLACEMENT_3D('',#9891,#5122,#5123) ;
#4225 = AXIS2_PLACEMENT_3D('',#9892,#5124,#5125) ;
#4226 = AXIS2_PLACEMENT_3D('',#9894,#5127,#5128) ;
#4227 = AXIS2_PLACEMENT_3D('',#9896,#5130,#5131) ;
#4228 = AXIS2_PLACEMENT_3D('',#9902,#5135,#5136) ;
#4229 = AXIS2_PLACEMENT_3D('',#9908,#5140,#5141) ;
#4230 = AXIS2_PLACEMENT_3D('',#9910,#5143,#5144) ;
#4231 = AXIS2_PLACEMENT_3D('',#9912,#5146,#5147) ;
#4232 = AXIS2_PLACEMENT_3D('',#9913,#5148,#5149) ;
#4233 = AXIS2_PLACEMENT_3D('',#9914,#5150,#5151) ;
#4234 = AXIS2_PLACEMENT_3D('',#9916,#5152,#5153) ;
#4235 = AXIS2_PLACEMENT_3D('',#9918,#5154,#5155) ;
#4236 = AXIS2_PLACEMENT_3D('',#9920,#5156,#5157) ;
#4237 = AXIS2_PLACEMENT_3D('',#9921,#5158,#5159) ;
#4238 = AXIS2_PLACEMENT_3D('',#9922,#5160,#5161) ;
#4239 = AXIS2_PLACEMENT_3D('',#9924,#5162,#5163) ;
#4240 = AXIS2_PLACEMENT_3D('',#9926,#5164,#5165) ;
#4241 = AXIS2_PLACEMENT_3D('',#9927,#5166,#5167) ;
#4242 = AXIS2_PLACEMENT_3D('',#9928,#5168,#5169) ;
#4243 = AXIS2_PLACEMENT_3D('',#9931,#5170,#5171) ;
#4244 = AXIS2_PLACEMENT_3D('',#9932,#5172,#5173) ;
#4245 = AXIS2_PLACEMENT_3D('',#9934,#5174,#5175) ;
#4246 = AXIS2_PLACEMENT_3D('',#9936,#5176,#5177) ;
#4247 = AXIS2_PLACEMENT_3D('',#9937,#5178,#5179) ;
#4248 = AXIS2_PLACEMENT_3D('',#9938,#5180,#5181) ;
#4249 = AXIS2_PLACEMENT_3D('',#9941,#5182,#5183) ;
#4250 = AXIS2_PLACEMENT_3D('',#9943,#5184,#5185) ;
#4251 = AXIS2_PLACEMENT_3D('',#9945,#5186,#5187) ;
#4252 = AXIS2_PLACEMENT_3D('',#9946,#5188,#5189) ;
#4253 = AXIS2_PLACEMENT_3D('',#9947,#5190,#5191) ;
#4254 = AXIS2_PLACEMENT_3D('',#9948,#5192,#5193) ;
#4255 = AXIS2_PLACEMENT_3D('',#9951,#5194,#5195) ;
#4256 = AXIS2_PLACEMENT_3D('',#9952,#5196,#5197) ;
#4257 = AXIS2_PLACEMENT_3D('',#9954,#5198,#5199) ;
#4258 = AXIS2_PLACEMENT_3D('',#9956,#5200,#5201) ;
#4259 = AXIS2_PLACEMENT_3D('',#9957,#5202,#5203) ;
#4260 = AXIS2_PLACEMENT_3D('',#9958,#5204,#5205) ;
#4261 = AXIS2_PLACEMENT_3D('',#9961,#5206,#5207) ;
#4262 = AXIS2_PLACEMENT_3D('',#9962,#5208,#5209) ;
#4263 = AXIS2_PLACEMENT_3D('',#9964,#5210,#5211) ;
#4264 = AXIS2_PLACEMENT_3D('',#9965,#5212,#5213) ;
#4265 = AXIS2_PLACEMENT_3D('',#9966,#5214,#5215) ;
#4266 = AXIS2_PLACEMENT_3D('',#9968,#5216,#5217) ;
#4267 = AXIS2_PLACEMENT_3D('',#9970,#5218,#5219) ;
#4268 = AXIS2_PLACEMENT_3D('',#9971,#5220,#5221) ;
#4269 = AXIS2_PLACEMENT_3D('',#9972,#5222,#5223) ;
#4270 = AXIS2_PLACEMENT_3D('',#9975,#5224,#5225) ;
#4271 = AXIS2_PLACEMENT_3D('',#9976,#5226,#5227) ;
#4272 = AXIS2_PLACEMENT_3D('',#9978,#5228,#5229) ;
#4273 = AXIS2_PLACEMENT_3D('',#9980,#5230,#5231) ;
#4274 = AXIS2_PLACEMENT_3D('',#9981,#5232,#5233) ;
#4275 = AXIS2_PLACEMENT_3D('',#9982,#5234,#5235) ;
#4276 = AXIS2_PLACEMENT_3D('',#9984,#5237,#5238) ;
#4277 = AXIS2_PLACEMENT_3D('',#9986,#5240,#5241) ;
#4278 = AXIS2_PLACEMENT_3D('',#9988,#5243,#5244) ;
#4279 = AXIS2_PLACEMENT_3D('',#9990,#5246,#5247) ;
#4280 = AXIS2_PLACEMENT_3D('',#9992,#5249,#5250) ;
#4281 = AXIS2_PLACEMENT_3D('',#9994,#5252,#5253) ;
#4282 = AXIS2_PLACEMENT_3D('',#9996,#5255,#5256) ;
#4283 = AXIS2_PLACEMENT_3D('',#9998,#5258,#5259) ;
#4284 = AXIS2_PLACEMENT_3D('',#9999,#5260,#5261) ;
#4285 = AXIS2_PLACEMENT_3D('',#10001,#5262,#5263) ;
#4286 = AXIS2_PLACEMENT_3D('',#10003,#5264,#5265) ;
#4287 = AXIS2_PLACEMENT_3D('',#10005,#5266,#5267) ;
#4288 = AXIS2_PLACEMENT_3D('',#10006,#5268,#5269) ;
#4289 = AXIS2_PLACEMENT_3D('',#10007,#5270,#5271) ;
#4290 = AXIS2_PLACEMENT_3D('',#10009,#5272,#5273) ;
#4291 = AXIS2_PLACEMENT_3D('',#10011,#5274,#5275) ;
#4292 = AXIS2_PLACEMENT_3D('',#10012,#5276,#5277) ;
#4293 = AXIS2_PLACEMENT_3D('',#10013,#5278,#5279) ;
#4294 = AXIS2_PLACEMENT_3D('',#10016,#5280,#5281) ;
#4295 = AXIS2_PLACEMENT_3D('',#10017,#5282,#5283) ;
#4296 = AXIS2_PLACEMENT_3D('',#10019,#5284,#5285) ;
#4297 = AXIS2_PLACEMENT_3D('',#10021,#5286,#5287) ;
#4298 = AXIS2_PLACEMENT_3D('',#10022,#5288,#5289) ;
#4299 = AXIS2_PLACEMENT_3D('',#10023,#5290,#5291) ;
#4300 = AXIS2_PLACEMENT_3D('',#10026,#5292,#5293) ;
#4301 = AXIS2_PLACEMENT_3D('',#10028,#5294,#5295) ;
#4302 = AXIS2_PLACEMENT_3D('',#10030,#5296,#5297) ;
#4303 = AXIS2_PLACEMENT_3D('',#10031,#5298,#5299) ;
#4304 = AXIS2_PLACEMENT_3D('',#10032,#5300,#5301) ;
#4305 = AXIS2_PLACEMENT_3D('',#10033,#5302,#5303) ;
#4306 = AXIS2_PLACEMENT_3D('',#10036,#5304,#5305) ;
#4307 = AXIS2_PLACEMENT_3D('',#10037,#5306,#5307) ;
#4308 = AXIS2_PLACEMENT_3D('',#10039,#5308,#5309) ;
#4309 = AXIS2_PLACEMENT_3D('',#10041,#5310,#5311) ;
#4310 = AXIS2_PLACEMENT_3D('',#10042,#5312,#5313) ;
#4311 = AXIS2_PLACEMENT_3D('',#10043,#5314,#5315) ;
#4312 = AXIS2_PLACEMENT_3D('',#10046,#5316,#5317) ;
#4313 = AXIS2_PLACEMENT_3D('',#10047,#5318,#5319) ;
#4314 = AXIS2_PLACEMENT_3D('',#10049,#5320,#5321) ;
#4315 = AXIS2_PLACEMENT_3D('',#10050,#5322,#5323) ;
#4316 = AXIS2_PLACEMENT_3D('',#10051,#5324,#5325) ;
#4317 = AXIS2_PLACEMENT_3D('',#10053,#5326,#5327) ;
#4318 = AXIS2_PLACEMENT_3D('',#10055,#5328,#5329) ;
#4319 = AXIS2_PLACEMENT_3D('',#10056,#5330,#5331) ;
#4320 = AXIS2_PLACEMENT_3D('',#10057,#5332,#5333) ;
#4321 = AXIS2_PLACEMENT_3D('',#10060,#5334,#5335) ;
#4322 = AXIS2_PLACEMENT_3D('',#10061,#5336,#5337) ;
#4323 = AXIS2_PLACEMENT_3D('',#10063,#5338,#5339) ;
#4324 = AXIS2_PLACEMENT_3D('',#10065,#5340,#5341) ;
#4325 = AXIS2_PLACEMENT_3D('',#10066,#5342,#5343) ;
#4326 = AXIS2_PLACEMENT_3D('',#10067,#5344,#5345) ;
#4327 = AXIS2_PLACEMENT_3D('',#10069,#5347,#5348) ;
#4328 = AXIS2_PLACEMENT_3D('',#10071,#5350,#5351) ;
#4329 = AXIS2_PLACEMENT_3D('',#10073,#5353,#5354) ;
#4330 = AXIS2_PLACEMENT_3D('',#10075,#5356,#5357) ;
#4331 = AXIS2_PLACEMENT_3D('',#10077,#5359,#5360) ;
#4332 = AXIS2_PLACEMENT_3D('',#10079,#5362,#5363) ;
#4333 = AXIS2_PLACEMENT_3D('',#10081,#5365,#5366) ;
#4334 = AXIS2_PLACEMENT_3D('',#10083,#5368,#5369) ;
#4335 = AXIS2_PLACEMENT_3D('',#10084,#5370,#5371) ;
#4336 = AXIS2_PLACEMENT_3D('',#10086,#5372,#5373) ;
#4337 = AXIS2_PLACEMENT_3D('',#10088,#5374,#5375) ;
#4338 = AXIS2_PLACEMENT_3D('',#10090,#5376,#5377) ;
#4339 = AXIS2_PLACEMENT_3D('',#10091,#5378,#5379) ;
#4340 = AXIS2_PLACEMENT_3D('',#10092,#5380,#5381) ;
#4341 = AXIS2_PLACEMENT_3D('',#10094,#5382,#5383) ;
#4342 = AXIS2_PLACEMENT_3D('',#10096,#5384,#5385) ;
#4343 = AXIS2_PLACEMENT_3D('',#10097,#5386,#5387) ;
#4344 = AXIS2_PLACEMENT_3D('',#10098,#5388,#5389) ;
#4345 = AXIS2_PLACEMENT_3D('',#10101,#5390,#5391) ;
#4346 = AXIS2_PLACEMENT_3D('',#10102,#5392,#5393) ;
#4347 = AXIS2_PLACEMENT_3D('',#10104,#5394,#5395) ;
#4348 = AXIS2_PLACEMENT_3D('',#10106,#5396,#5397) ;
#4349 = AXIS2_PLACEMENT_3D('',#10107,#5398,#5399) ;
#4350 = AXIS2_PLACEMENT_3D('',#10108,#5400,#5401) ;
#4351 = AXIS2_PLACEMENT_3D('',#10111,#5402,#5403) ;
#4352 = AXIS2_PLACEMENT_3D('',#10113,#5404,#5405) ;
#4353 = AXIS2_PLACEMENT_3D('',#10115,#5406,#5407) ;
#4354 = AXIS2_PLACEMENT_3D('',#10116,#5408,#5409) ;
#4355 = AXIS2_PLACEMENT_3D('',#10117,#5410,#5411) ;
#4356 = AXIS2_PLACEMENT_3D('',#10118,#5412,#5413) ;
#4357 = AXIS2_PLACEMENT_3D('',#10121,#5414,#5415) ;
#4358 = AXIS2_PLACEMENT_3D('',#10122,#5416,#5417) ;
#4359 = AXIS2_PLACEMENT_3D('',#10124,#5418,#5419) ;
#4360 = AXIS2_PLACEMENT_3D('',#10126,#5420,#5421) ;
#4361 = AXIS2_PLACEMENT_3D('',#10127,#5422,#5423) ;
#4362 = AXIS2_PLACEMENT_3D('',#10128,#5424,#5425) ;
#4363 = AXIS2_PLACEMENT_3D('',#10131,#5426,#5427) ;
#4364 = AXIS2_PLACEMENT_3D('',#10132,#5428,#5429) ;
#4365 = AXIS2_PLACEMENT_3D('',#10134,#5430,#5431) ;
#4366 = AXIS2_PLACEMENT_3D('',#10135,#5432,#5433) ;
#4367 = AXIS2_PLACEMENT_3D('',#10136,#5434,#5435) ;
#4368 = AXIS2_PLACEMENT_3D('',#10138,#5436,#5437) ;
#4369 = AXIS2_PLACEMENT_3D('',#10140,#5438,#5439) ;
#4370 = AXIS2_PLACEMENT_3D('',#10141,#5440,#5441) ;
#4371 = AXIS2_PLACEMENT_3D('',#10142,#5442,#5443) ;
#4372 = AXIS2_PLACEMENT_3D('',#10145,#5444,#5445) ;
#4373 = AXIS2_PLACEMENT_3D('',#10146,#5446,#5447) ;
#4374 = AXIS2_PLACEMENT_3D('',#10148,#5448,#5449) ;
#4375 = AXIS2_PLACEMENT_3D('',#10150,#5450,#5451) ;
#4376 = AXIS2_PLACEMENT_3D('',#10151,#5452,#5453) ;
#4377 = AXIS2_PLACEMENT_3D('',#10152,#5454,#5455) ;
#4378 = AXIS2_PLACEMENT_3D('',#10154,#5457,#5458) ;
#4379 = AXIS2_PLACEMENT_3D('',#10156,#5460,#5461) ;
#4380 = AXIS2_PLACEMENT_3D('',#10158,#5463,#5464) ;
#4381 = AXIS2_PLACEMENT_3D('',#10160,#5466,#5467) ;
#4382 = AXIS2_PLACEMENT_3D('',#10162,#5469,#5470) ;
#4383 = AXIS2_PLACEMENT_3D('',#10164,#5472,#5473) ;
#4384 = AXIS2_PLACEMENT_3D('',#10166,#5475,#5476) ;
#4385 = AXIS2_PLACEMENT_3D('',#10168,#5478,#5479) ;
#4386 = AXIS2_PLACEMENT_3D('',#10169,#5480,#5481) ;
#4387 = AXIS2_PLACEMENT_3D('',#10171,#5482,#5483) ;
#4388 = AXIS2_PLACEMENT_3D('',#10173,#5484,#5485) ;
#4389 = AXIS2_PLACEMENT_3D('',#10175,#5486,#5487) ;
#4390 = AXIS2_PLACEMENT_3D('',#10176,#5488,#5489) ;
#4391 = AXIS2_PLACEMENT_3D('',#10177,#5490,#5491) ;
#4392 = AXIS2_PLACEMENT_3D('',#10179,#5492,#5493) ;
#4393 = AXIS2_PLACEMENT_3D('',#10181,#5494,#5495) ;
#4394 = AXIS2_PLACEMENT_3D('',#10182,#5496,#5497) ;
#4395 = AXIS2_PLACEMENT_3D('',#10183,#5498,#5499) ;
#4396 = AXIS2_PLACEMENT_3D('',#10186,#5500,#5501) ;
#4397 = AXIS2_PLACEMENT_3D('',#10187,#5502,#5503) ;
#4398 = AXIS2_PLACEMENT_3D('',#10189,#5504,#5505) ;
#4399 = AXIS2_PLACEMENT_3D('',#10191,#5506,#5507) ;
#4400 = AXIS2_PLACEMENT_3D('',#10192,#5508,#5509) ;
#4401 = AXIS2_PLACEMENT_3D('',#10193,#5510,#5511) ;
#4402 = AXIS2_PLACEMENT_3D('',#10196,#5512,#5513) ;
#4403 = AXIS2_PLACEMENT_3D('',#10198,#5514,#5515) ;
#4404 = AXIS2_PLACEMENT_3D('',#10200,#5516,#5517) ;
#4405 = AXIS2_PLACEMENT_3D('',#10201,#5518,#5519) ;
#4406 = AXIS2_PLACEMENT_3D('',#10202,#5520,#5521) ;
#4407 = AXIS2_PLACEMENT_3D('',#10203,#5522,#5523) ;
#4408 = AXIS2_PLACEMENT_3D('',#10206,#5524,#5525) ;
#4409 = AXIS2_PLACEMENT_3D('',#10207,#5526,#5527) ;
#4410 = AXIS2_PLACEMENT_3D('',#10209,#5528,#5529) ;
#4411 = AXIS2_PLACEMENT_3D('',#10211,#5530,#5531) ;
#4412 = AXIS2_PLACEMENT_3D('',#10212,#5532,#5533) ;
#4413 = AXIS2_PLACEMENT_3D('',#10213,#5534,#5535) ;
#4414 = AXIS2_PLACEMENT_3D('',#10216,#5536,#5537) ;
#4415 = AXIS2_PLACEMENT_3D('',#10217,#5538,#5539) ;
#4416 = AXIS2_PLACEMENT_3D('',#10219,#5540,#5541) ;
#4417 = AXIS2_PLACEMENT_3D('',#10220,#5542,#5543) ;
#4418 = AXIS2_PLACEMENT_3D('',#10221,#5544,#5545) ;
#4419 = AXIS2_PLACEMENT_3D('',#10223,#5546,#5547) ;
#4420 = AXIS2_PLACEMENT_3D('',#10225,#5548,#5549) ;
#4421 = AXIS2_PLACEMENT_3D('',#10226,#5550,#5551) ;
#4422 = AXIS2_PLACEMENT_3D('',#10227,#5552,#5553) ;
#4423 = AXIS2_PLACEMENT_3D('',#10230,#5554,#5555) ;
#4424 = AXIS2_PLACEMENT_3D('',#10231,#5556,#5557) ;
#4425 = AXIS2_PLACEMENT_3D('',#10233,#5558,#5559) ;
#4426 = AXIS2_PLACEMENT_3D('',#10235,#5560,#5561) ;
#4427 = AXIS2_PLACEMENT_3D('',#10236,#5562,#5563) ;
#4428 = AXIS2_PLACEMENT_3D('',#10237,#5564,#5565) ;
#4429 = AXIS2_PLACEMENT_3D('',#10239,#5567,#5568) ;
#4430 = AXIS2_PLACEMENT_3D('',#10241,#5570,#5571) ;
#4431 = AXIS2_PLACEMENT_3D('',#10243,#5573,#5574) ;
#4432 = AXIS2_PLACEMENT_3D('',#10245,#5576,#5577) ;
#4433 = AXIS2_PLACEMENT_3D('',#10247,#5579,#5580) ;
#4434 = AXIS2_PLACEMENT_3D('',#10249,#5582,#5583) ;
#4435 = AXIS2_PLACEMENT_3D('',#10251,#5585,#5586) ;
#4436 = AXIS2_PLACEMENT_3D('',#10253,#5588,#5589) ;
#4437 = AXIS2_PLACEMENT_3D('',#10254,#5590,#5591) ;
#4438 = AXIS2_PLACEMENT_3D('',#10255,#5592,#5593) ;
#4439 = AXIS2_PLACEMENT_3D('',#10256,#5594,#5595) ;
#4440 = AXIS2_PLACEMENT_3D('',#10257,#5596,#5597) ;
#4441 = AXIS2_PLACEMENT_3D('',#10258,#5598,#5599) ;
#4442 = AXIS2_PLACEMENT_3D('',#10259,#5600,#5601) ;
#4443 = AXIS2_PLACEMENT_3D('',#10260,#5602,#5603) ;
#4444 = DIRECTION('axis',(0.,0.,1.)) ;
#4445 = DIRECTION('refdir',(1.,0.,0.)) ;
#4446 = DIRECTION('axis',(0.,0.,1.)) ;
#4447 = DIRECTION('refdir',(1.,0.,0.)) ;
#4448 = DIRECTION('axis',(0.,0.,1.)) ;
#4449 = DIRECTION('refdir',(1.,0.,0.)) ;
#4450 = DIRECTION('center_axis',(0.,-1.,0.)) ;
#4451 = DIRECTION('ref_axis',(0.,0.,-1.)) ;
#4452 = DIRECTION('center_axis',(0.,-1.,0.)) ;
#4453 = DIRECTION('ref_axis',(0.,0.,-1.)) ;
#4454 = DIRECTION('center_axis',(0.,-1.,0.)) ;
#4455 = DIRECTION('ref_axis',(0.,0.,-1.)) ;
#4456 = DIRECTION('center_axis',(1.,0.,1.44280892518809E-16)) ;
#4457 = DIRECTION('ref_axis',(-1.44280892518809E-16,0.,1.)) ;
#4458 = DIRECTION('center_axis',(0.,-1.,0.)) ;
#4459 = DIRECTION('ref_axis',(0.,0.,-1.)) ;
#4460 = DIRECTION('center_axis',(0.,-1.,0.)) ;
#4461 = DIRECTION('ref_axis',(0.,0.,-1.)) ;
#4462 = DIRECTION('center_axis',(0.,-1.,0.)) ;
#4463 = DIRECTION('ref_axis',(0.,0.,-1.)) ;
#4464 = DIRECTION('center_axis',(-1.,0.,-1.43842767649164E-16)) ;
#4465 = DIRECTION('ref_axis',(-1.43842767649164E-16,0.,1.)) ;
#4466 = DIRECTION('center_axis',(0.,-1.,0.)) ;
#4467 = DIRECTION('ref_axis',(0.,0.,-1.)) ;
#4468 = DIRECTION('center_axis',(0.,-1.,0.)) ;
#4469 = DIRECTION('ref_axis',(0.,0.,-1.)) ;
#4470 = DIRECTION('center_axis',(0.,1.,0.)) ;
#4471 = DIRECTION('ref_axis',(0.,0.,1.)) ;
#4472 = DIRECTION('',(8.89414010481862E-17,-0.687418365521554,0.726261654463235)) ;
#4473 = DIRECTION('center_axis',(0.,-1.,0.)) ;
#4474 = DIRECTION('ref_axis',(0.,0.,-1.)) ;
#4475 = DIRECTION('axis',(0.,0.,1.)) ;
#4476 = DIRECTION('refdir',(1.,0.,0.)) ;
#4477 = DIRECTION('center_axis',(0.,-1.,0.)) ;
#4478 = DIRECTION('ref_axis',(0.,0.,-1.)) ;
#4479 = DIRECTION('center_axis',(0.,-1.,0.)) ;
#4480 = DIRECTION('ref_axis',(0.,0.,-1.)) ;
#4481 = DIRECTION('center_axis',(0.,-1.,0.)) ;
#4482 = DIRECTION('ref_axis',(0.,0.,-1.)) ;
#4483 = DIRECTION('center_axis',(1.,0.,1.20984279938742E-16)) ;
#4484 = DIRECTION('ref_axis',(-1.20984279938742E-16,0.,1.)) ;
#4485 = DIRECTION('center_axis',(0.,-1.,0.)) ;
#4486 = DIRECTION('ref_axis',(0.,0.,-1.)) ;
#4487 = DIRECTION('center_axis',(0.,-1.,0.)) ;
#4488 = DIRECTION('ref_axis',(0.,0.,-1.)) ;
#4489 = DIRECTION('center_axis',(0.,1.,0.)) ;
#4490 = DIRECTION('ref_axis',(0.,0.,1.)) ;
#4491 = DIRECTION('',(4.9528867173767E-17,-0.914567234661089,0.404433892353705)) ;
#4492 = DIRECTION('center_axis',(0.,-1.,0.)) ;
#4493 = DIRECTION('ref_axis',(0.,0.,-1.)) ;
#4494 = DIRECTION('center_axis',(0.,-1.,0.)) ;
#4495 = DIRECTION('ref_axis',(0.,0.,-1.)) ;
#4496 = DIRECTION('center_axis',(0.,-1.,0.)) ;
#4497 = DIRECTION('ref_axis',(0.,0.,-1.)) ;
#4498 = DIRECTION('center_axis',(0.,-1.,0.)) ;
#4499 = DIRECTION('ref_axis',(0.,0.,-1.)) ;
#4500 = DIRECTION('center_axis',(0.,-1.,0.)) ;
#4501 = DIRECTION('ref_axis',(0.,0.,-1.)) ;
#4502 = DIRECTION('center_axis',(-1.,0.,-1.20676066801522E-16)) ;
#4503 = DIRECTION('ref_axis',(-1.20676066801522E-16,0.,1.)) ;
#4504 = DIRECTION('center_axis',(0.,1.,0.)) ;
#4505 = DIRECTION('ref_axis',(0.,0.,1.)) ;
#4506 = DIRECTION('',(-8.89414010484684E-17,0.687418365519119,-0.72626165446554)) ;
#4507 = DIRECTION('axis',(0.,0.,1.)) ;
#4508 = DIRECTION('refdir',(1.,0.,0.)) ;
#4509 = DIRECTION('center_axis',(6.42891162084177E-17,1.,1.01883556321148E-16)) ;
#4510 = DIRECTION('ref_axis',(-1.,0.,0.)) ;
#4511 = DIRECTION('center_axis',(0.,1.01883556321148E-16,-1.)) ;
#4512 = DIRECTION('ref_axis',(1.,0.,0.)) ;
#4513 = DIRECTION('center_axis',(-6.42891162084177E-17,-1.,-1.01883556321148E-16)) ;
#4514 = DIRECTION('ref_axis',(-1.,6.42891162084177E-17,6.55000379205715E-33)) ;
#4515 = DIRECTION('axis',(0.,0.,1.)) ;
#4516 = DIRECTION('refdir',(1.,0.,0.)) ;
#4517 = DIRECTION('center_axis',(6.42891162084177E-17,1.,1.01883556321148E-16)) ;
#4518 = DIRECTION('ref_axis',(-1.,0.,0.)) ;
#4519 = DIRECTION('center_axis',(0.,1.01883556321148E-16,-1.)) ;
#4520 = DIRECTION('ref_axis',(1.,0.,0.)) ;
#4521 = DIRECTION('center_axis',(-6.42891162084177E-17,-1.,-1.01883556321148E-16)) ;
#4522 = DIRECTION('ref_axis',(-1.,6.42891162084177E-17,6.55000379205715E-33)) ;
#4523 = DIRECTION('axis',(0.,0.,1.)) ;
#4524 = DIRECTION('refdir',(1.,0.,0.)) ;
#4525 = DIRECTION('center_axis',(6.42891162084177E-17,1.,1.01883556321148E-16)) ;
#4526 = DIRECTION('ref_axis',(-1.,0.,0.)) ;
#4527 = DIRECTION('center_axis',(0.,1.01883556321148E-16,-1.)) ;
#4528 = DIRECTION('ref_axis',(1.,0.,0.)) ;
#4529 = DIRECTION('center_axis',(-6.42891162084177E-17,-1.,-1.01883556321148E-16)) ;
#4530 = DIRECTION('ref_axis',(-1.,6.42891162084177E-17,6.55000379205715E-33)) ;
#4531 = DIRECTION('axis',(0.,0.,1.)) ;
#4532 = DIRECTION('refdir',(1.,0.,0.)) ;
#4533 = DIRECTION('center_axis',(6.42891162084177E-17,1.,1.01883556321148E-16)) ;
#4534 = DIRECTION('ref_axis',(-1.,0.,0.)) ;
#4535 = DIRECTION('center_axis',(0.,1.01883556321148E-16,-1.)) ;
#4536 = DIRECTION('ref_axis',(1.,0.,0.)) ;
#4537 = DIRECTION('center_axis',(-6.42891162084177E-17,-1.,-1.01883556321148E-16)) ;
#4538 = DIRECTION('ref_axis',(-1.,6.42891162084177E-17,6.55000379205715E-33)) ;
#4539 = DIRECTION('axis',(0.,0.,1.)) ;
#4540 = DIRECTION('refdir',(1.,0.,0.)) ;
#4541 = DIRECTION('center_axis',(6.42891162084177E-17,1.,1.01883556321148E-16)) ;
#4542 = DIRECTION('ref_axis',(-1.,0.,0.)) ;
#4543 = DIRECTION('center_axis',(0.,1.01883556321148E-16,-1.)) ;
#4544 = DIRECTION('ref_axis',(1.,0.,0.)) ;
#4545 = DIRECTION('center_axis',(-6.42891162084177E-17,-1.,-1.01883556321148E-16)) ;
#4546 = DIRECTION('ref_axis',(-1.,6.42891162084177E-17,6.55000379205715E-33)) ;
#4547 = DIRECTION('axis',(0.,0.,1.)) ;
#4548 = DIRECTION('refdir',(1.,0.,0.)) ;
#4549 = DIRECTION('center_axis',(-6.42891162084177E-17,-1.,-1.01883556321148E-16)) ;
#4550 = DIRECTION('ref_axis',(1.,0.,0.)) ;
#4551 = DIRECTION('center_axis',(0.,1.01883556321148E-16,-1.)) ;
#4552 = DIRECTION('ref_axis',(-1.,0.,0.)) ;
#4553 = DIRECTION('center_axis',(6.42891162084177E-17,1.,1.01883556321148E-16)) ;
#4554 = DIRECTION('ref_axis',(1.,-6.42891162084177E-17,-6.55000379205715E-33)) ;
#4555 = DIRECTION('axis',(0.,0.,1.)) ;
#4556 = DIRECTION('refdir',(1.,0.,0.)) ;
#4557 = DIRECTION('center_axis',(-6.42891162084177E-17,-1.,-1.01883556321148E-16)) ;
#4558 = DIRECTION('ref_axis',(1.,0.,0.)) ;
#4559 = DIRECTION('center_axis',(0.,1.01883556321148E-16,-1.)) ;
#4560 = DIRECTION('ref_axis',(-1.,0.,0.)) ;
#4561 = DIRECTION('center_axis',(6.42891162084177E-17,1.,1.01883556321148E-16)) ;
#4562 = DIRECTION('ref_axis',(1.,-6.42891162084177E-17,-6.55000379205715E-33)) ;
#4563 = DIRECTION('axis',(0.,0.,1.)) ;
#4564 = DIRECTION('refdir',(1.,0.,0.)) ;
#4565 = DIRECTION('center_axis',(-6.42891162084177E-17,-1.,-1.01883556321148E-16)) ;
#4566 = DIRECTION('ref_axis',(1.,0.,0.)) ;
#4567 = DIRECTION('center_axis',(0.,1.01883556321148E-16,-1.)) ;
#4568 = DIRECTION('ref_axis',(-1.,0.,0.)) ;
#4569 = DIRECTION('center_axis',(6.42891162084177E-17,1.,1.01883556321148E-16)) ;
#4570 = DIRECTION('ref_axis',(1.,-6.42891162084177E-17,-6.55000379205715E-33)) ;
#4571 = DIRECTION('axis',(0.,0.,1.)) ;
#4572 = DIRECTION('refdir',(1.,0.,0.)) ;
#4573 = DIRECTION('center_axis',(-6.42891162084177E-17,-1.,-1.01883556321148E-16)) ;
#4574 = DIRECTION('ref_axis',(1.,0.,0.)) ;
#4575 = DIRECTION('center_axis',(0.,1.01883556321148E-16,-1.)) ;
#4576 = DIRECTION('ref_axis',(-1.,0.,0.)) ;
#4577 = DIRECTION('center_axis',(6.42891162084177E-17,1.,1.01883556321148E-16)) ;
#4578 = DIRECTION('ref_axis',(1.,-6.42891162084177E-17,-6.55000379205715E-33)) ;
#4579 = DIRECTION('axis',(0.,0.,1.)) ;
#4580 = DIRECTION('refdir',(1.,0.,0.)) ;
#4581 = DIRECTION('center_axis',(-6.42891162084177E-17,-1.,-1.01883556321148E-16)) ;
#4582 = DIRECTION('ref_axis',(1.,0.,0.)) ;
#4583 = DIRECTION('center_axis',(0.,1.01883556321148E-16,-1.)) ;
#4584 = DIRECTION('ref_axis',(-1.,0.,0.)) ;
#4585 = DIRECTION('center_axis',(6.42891162084177E-17,1.,1.01883556321148E-16)) ;
#4586 = DIRECTION('ref_axis',(1.,-6.42891162084177E-17,-6.55000379205715E-33)) ;
#4587 = DIRECTION('axis',(0.,0.,1.)) ;
#4588 = DIRECTION('refdir',(1.,0.,0.)) ;
#4589 = DIRECTION('center_axis',(-6.42891162084177E-17,-1.,-1.01883556321148E-16)) ;
#4590 = DIRECTION('ref_axis',(1.,0.,0.)) ;
#4591 = DIRECTION('center_axis',(0.,1.01883556321148E-16,-1.)) ;
#4592 = DIRECTION('ref_axis',(-1.,0.,0.)) ;
#4593 = DIRECTION('center_axis',(6.42891162084177E-17,1.,1.01883556321148E-16)) ;
#4594 = DIRECTION('ref_axis',(1.,-6.42891162084177E-17,-6.55000379205715E-33)) ;
#4595 = DIRECTION('axis',(0.,0.,1.)) ;
#4596 = DIRECTION('refdir',(1.,0.,0.)) ;
#4597 = DIRECTION('center_axis',(-6.42891162084177E-17,-1.,-1.01883556321148E-16)) ;
#4598 = DIRECTION('ref_axis',(1.,0.,0.)) ;
#4599 = DIRECTION('center_axis',(0.,1.01883556321148E-16,-1.)) ;
#4600 = DIRECTION('ref_axis',(-1.,0.,0.)) ;
#4601 = DIRECTION('center_axis',(6.42891162084177E-17,1.,1.01883556321148E-16)) ;
#4602 = DIRECTION('ref_axis',(1.,-6.42891162084177E-17,-6.55000379205715E-33)) ;
#4603 = DIRECTION('axis',(0.,0.,1.)) ;
#4604 = DIRECTION('refdir',(1.,0.,0.)) ;
#4605 = DIRECTION('center_axis',(-6.42891162084177E-17,-1.,-1.01883556321148E-16)) ;
#4606 = DIRECTION('ref_axis',(1.,0.,0.)) ;
#4607 = DIRECTION('center_axis',(0.,1.01883556321148E-16,-1.)) ;
#4608 = DIRECTION('ref_axis',(-1.,0.,0.)) ;
#4609 = DIRECTION('center_axis',(6.42891162084177E-17,1.,1.01883556321148E-16)) ;
#4610 = DIRECTION('ref_axis',(1.,-6.42891162084177E-17,-6.55000379205715E-33)) ;
#4611 = DIRECTION('axis',(0.,0.,1.)) ;
#4612 = DIRECTION('refdir',(1.,0.,0.)) ;
#4613 = DIRECTION('center_axis',(-6.42891162084177E-17,-1.,-1.01883556321148E-16)) ;
#4614 = DIRECTION('ref_axis',(1.,0.,0.)) ;
#4615 = DIRECTION('center_axis',(0.,1.01883556321148E-16,-1.)) ;
#4616 = DIRECTION('ref_axis',(-1.,0.,0.)) ;
#4617 = DIRECTION('center_axis',(6.42891162084177E-17,1.,1.01883556321148E-16)) ;
#4618 = DIRECTION('ref_axis',(1.,-6.42891162084177E-17,-6.55000379205715E-33)) ;
#4619 = DIRECTION('axis',(0.,0.,1.)) ;
#4620 = DIRECTION('refdir',(1.,0.,0.)) ;
#4621 = DIRECTION('center_axis',(-6.42891162084177E-17,-1.,-1.01883556321148E-16)) ;
#4622 = DIRECTION('ref_axis',(1.,0.,0.)) ;
#4623 = DIRECTION('center_axis',(0.,1.01883556321148E-16,-1.)) ;
#4624 = DIRECTION('ref_axis',(-1.,0.,0.)) ;
#4625 = DIRECTION('center_axis',(6.42891162084177E-17,1.,1.01883556321148E-16)) ;
#4626 = DIRECTION('ref_axis',(1.,-6.42891162084177E-17,-6.55000379205715E-33)) ;
#4627 = DIRECTION('axis',(0.,0.,1.)) ;
#4628 = DIRECTION('refdir',(1.,0.,0.)) ;
#4629 = DIRECTION('center_axis',(-6.42891162084177E-17,-1.,-1.01883556321148E-16)) ;
#4630 = DIRECTION('ref_axis',(1.,0.,0.)) ;
#4631 = DIRECTION('center_axis',(0.,1.01883556321148E-16,-1.)) ;
#4632 = DIRECTION('ref_axis',(-1.,0.,0.)) ;
#4633 = DIRECTION('center_axis',(6.42891162084177E-17,1.,1.01883556321148E-16)) ;
#4634 = DIRECTION('ref_axis',(1.,-6.42891162084177E-17,-6.55000379205715E-33)) ;
#4635 = DIRECTION('axis',(0.,0.,1.)) ;
#4636 = DIRECTION('refdir',(1.,0.,0.)) ;
#4637 = DIRECTION('center_axis',(-6.42891162084177E-17,-1.,-1.01883556321148E-16)) ;
#4638 = DIRECTION('ref_axis',(1.,0.,0.)) ;
#4639 = DIRECTION('center_axis',(0.,1.01883556321148E-16,-1.)) ;
#4640 = DIRECTION('ref_axis',(-1.,0.,0.)) ;
#4641 = DIRECTION('center_axis',(6.42891162084177E-17,1.,1.01883556321148E-16)) ;
#4642 = DIRECTION('ref_axis',(1.,-6.42891162084177E-17,-6.55000379205715E-33)) ;
#4643 = DIRECTION('axis',(0.,0.,1.)) ;
#4644 = DIRECTION('refdir',(1.,0.,0.)) ;
#4645 = DIRECTION('center_axis',(-6.42891162084177E-17,-1.,-1.01883556321148E-16)) ;
#4646 = DIRECTION('ref_axis',(1.,0.,0.)) ;
#4647 = DIRECTION('center_axis',(0.,1.01883556321148E-16,-1.)) ;
#4648 = DIRECTION('ref_axis',(-1.,0.,0.)) ;
#4649 = DIRECTION('center_axis',(6.42891162084177E-17,1.,1.01883556321148E-16)) ;
#4650 = DIRECTION('ref_axis',(1.,-6.42891162084177E-17,-6.55000379205715E-33)) ;
#4651 = DIRECTION('axis',(0.,0.,1.)) ;
#4652 = DIRECTION('refdir',(1.,0.,0.)) ;
#4653 = DIRECTION('center_axis',(-6.42891162084177E-17,-1.,-1.01883556321148E-16)) ;
#4654 = DIRECTION('ref_axis',(1.,0.,0.)) ;
#4655 = DIRECTION('center_axis',(0.,1.01883556321148E-16,-1.)) ;
#4656 = DIRECTION('ref_axis',(-1.,0.,0.)) ;
#4657 = DIRECTION('center_axis',(6.42891162084177E-17,1.,1.01883556321148E-16)) ;
#4658 = DIRECTION('ref_axis',(1.,-6.42891162084177E-17,-6.55000379205715E-33)) ;
#4659 = DIRECTION('axis',(0.,0.,1.)) ;
#4660 = DIRECTION('refdir',(1.,0.,0.)) ;
#4661 = DIRECTION('center_axis',(-6.42891162084177E-17,-1.,-1.01883556321148E-16)) ;
#4662 = DIRECTION('ref_axis',(1.,0.,0.)) ;
#4663 = DIRECTION('center_axis',(0.,1.01883556321148E-16,-1.)) ;
#4664 = DIRECTION('ref_axis',(-1.,0.,0.)) ;
#4665 = DIRECTION('center_axis',(6.42891162084177E-17,1.,1.01883556321148E-16)) ;
#4666 = DIRECTION('ref_axis',(1.,-6.42891162084177E-17,-6.55000379205715E-33)) ;
#4667 = DIRECTION('axis',(0.,0.,1.)) ;
#4668 = DIRECTION('refdir',(1.,0.,0.)) ;
#4669 = DIRECTION('center_axis',(-6.42891162084177E-17,-1.,-1.01883556321148E-16)) ;
#4670 = DIRECTION('ref_axis',(1.,0.,0.)) ;
#4671 = DIRECTION('center_axis',(0.,1.01883556321148E-16,-1.)) ;
#4672 = DIRECTION('ref_axis',(-1.,0.,0.)) ;
#4673 = DIRECTION('center_axis',(6.42891162084177E-17,1.,1.01883556321148E-16)) ;
#4674 = DIRECTION('ref_axis',(1.,-6.42891162084177E-17,-6.55000379205715E-33)) ;
#4675 = DIRECTION('axis',(0.,0.,1.)) ;
#4676 = DIRECTION('refdir',(1.,0.,0.)) ;
#4677 = DIRECTION('center_axis',(-6.42891162084177E-17,-1.,-1.01883556321148E-16)) ;
#4678 = DIRECTION('ref_axis',(1.,0.,0.)) ;
#4679 = DIRECTION('center_axis',(0.,1.01883556321148E-16,-1.)) ;
#4680 = DIRECTION('ref_axis',(-1.,0.,0.)) ;
#4681 = DIRECTION('center_axis',(6.42891162084177E-17,1.,1.01883556321148E-16)) ;
#4682 = DIRECTION('ref_axis',(1.,-6.42891162084177E-17,-6.55000379205715E-33)) ;
#4683 = DIRECTION('',(0.,0.,1.)) ;
#4684 = DIRECTION('',(1.,0.,0.)) ;
#4685 = DIRECTION('',(0.,0.,1.)) ;
#4686 = DIRECTION('',(1.,0.,0.)) ;
#4687 = DIRECTION('',(0.,0.,1.)) ;
#4688 = DIRECTION('',(1.,0.,0.)) ;
#4689 = DIRECTION('',(0.,0.,1.)) ;
#4690 = DIRECTION('',(1.,0.,0.)) ;
#4691 = DIRECTION('',(0.,0.,1.)) ;
#4692 = DIRECTION('',(1.,0.,0.)) ;
#4693 = DIRECTION('',(0.,0.,1.)) ;
#4694 = DIRECTION('',(1.,0.,0.)) ;
#4695 = DIRECTION('',(0.,0.,1.)) ;
#4696 = DIRECTION('',(1.,0.,0.)) ;
#4697 = DIRECTION('',(0.,0.,1.)) ;
#4698 = DIRECTION('',(1.,0.,0.)) ;
#4699 = DIRECTION('',(0.,0.,1.)) ;
#4700 = DIRECTION('',(1.,0.,0.)) ;
#4701 = DIRECTION('',(0.,0.,1.)) ;
#4702 = DIRECTION('',(1.,0.,0.)) ;
#4703 = DIRECTION('',(0.,0.,1.)) ;
#4704 = DIRECTION('',(1.,0.,0.)) ;
#4705 = DIRECTION('',(0.,0.,1.)) ;
#4706 = DIRECTION('',(1.,0.,0.)) ;
#4707 = DIRECTION('',(0.,0.,1.)) ;
#4708 = DIRECTION('',(1.,0.,0.)) ;
#4709 = DIRECTION('',(0.,0.,1.)) ;
#4710 = DIRECTION('',(1.,0.,0.)) ;
#4711 = DIRECTION('',(0.,0.,1.)) ;
#4712 = DIRECTION('',(1.,0.,0.)) ;
#4713 = DIRECTION('',(0.,0.,1.)) ;
#4714 = DIRECTION('',(1.,0.,0.)) ;
#4715 = DIRECTION('',(0.,0.,1.)) ;
#4716 = DIRECTION('',(1.,0.,0.)) ;
#4717 = DIRECTION('',(0.,0.,1.)) ;
#4718 = DIRECTION('',(1.,0.,0.)) ;
#4719 = DIRECTION('',(0.,0.,1.)) ;
#4720 = DIRECTION('',(1.,0.,0.)) ;
#4721 = DIRECTION('',(0.,0.,1.)) ;
#4722 = DIRECTION('',(1.,0.,0.)) ;
#4723 = DIRECTION('',(0.,0.,1.)) ;
#4724 = DIRECTION('',(1.,0.,0.)) ;
#4725 = DIRECTION('',(0.,0.,1.)) ;
#4726 = DIRECTION('',(1.,0.,0.)) ;
#4727 = DIRECTION('',(0.,0.,1.)) ;
#4728 = DIRECTION('',(1.,0.,0.)) ;
#4729 = DIRECTION('',(0.,0.,1.)) ;
#4730 = DIRECTION('',(1.,0.,0.)) ;
#4731 = DIRECTION('axis',(0.,0.,1.)) ;
#4732 = DIRECTION('refdir',(1.,0.,0.)) ;
#4733 = DIRECTION('axis',(0.,0.,1.)) ;
#4734 = DIRECTION('refdir',(1.,0.,0.)) ;
#4735 = DIRECTION('center_axis',(6.42891162084177E-17,1.,1.01883556321148E-16)) ;
#4736 = DIRECTION('ref_axis',(-1.,6.42891162084177E-17,6.55000379205717E-33)) ;
#4737 = DIRECTION('center_axis',(6.42891162084177E-17,1.,1.01883556321148E-16)) ;
#4738 = DIRECTION('ref_axis',(-0.309016994374945,-7.70305906808054E-17,0.951056516295154)) ;
#4739 = DIRECTION('',(-6.42891162084177E-17,-1.,-1.01883556321148E-16)) ;
#4740 = DIRECTION('center_axis',(6.42891162084177E-17,1.,1.01883556321148E-16)) ;
#4741 = DIRECTION('ref_axis',(-1.,6.42891162084177E-17,6.55000379205717E-33)) ;
#4742 = DIRECTION('',(-6.42891162084177E-17,-1.,-1.01883556321148E-16)) ;
#4743 = DIRECTION('center_axis',(6.42891162084177E-17,1.,1.01883556321148E-16)) ;
#4744 = DIRECTION('ref_axis',(-1.,6.42891162084177E-17,6.55000379205717E-33)) ;
#4745 = DIRECTION('center_axis',(6.42891162084177E-17,1.,1.01883556321148E-16)) ;
#4746 = DIRECTION('ref_axis',(-1.,6.42891162084177E-17,6.55000379205717E-33)) ;
#4747 = DIRECTION('',(6.42891162084177E-17,1.,1.01883556321148E-16)) ;
#4748 = DIRECTION('',(6.42891162084177E-17,1.,1.01883556321148E-16)) ;
#4749 = DIRECTION('center_axis',(6.42891162084177E-17,1.,1.01883556321148E-16)) ;
#4750 = DIRECTION('ref_axis',(0.809016994374942,7.87466429072571E-18,-0.587785252292481)) ;
#4751 = DIRECTION('',(6.42891162084177E-17,1.,1.01883556321148E-16)) ;
#4752 = DIRECTION('center_axis',(6.42891162084177E-17,1.,1.01883556321148E-16)) ;
#4753 = DIRECTION('ref_axis',(-0.309016994374945,-7.70305906808054E-17,0.951056516295154)) ;
#4754 = DIRECTION('',(6.42891162084177E-17,1.,1.01883556321148E-16)) ;
#4755 = DIRECTION('center_axis',(6.42891162084177E-17,1.,1.01883556321148E-16)) ;
#4756 = DIRECTION('ref_axis',(0.809016994374951,-1.11896639422636E-16,0.587785252292469)) ;
#4757 = DIRECTION('',(6.42891162084177E-17,1.,1.01883556321148E-16)) ;
#4758 = DIRECTION('center_axis',(6.42891162084177E-17,1.,1.01883556321148E-16)) ;
#4759 = DIRECTION('ref_axis',(-0.309016994374958,1.16763449604299E-16,-0.95105651629515)) ;
#4760 = DIRECTION('center_axis',(6.42891162084176E-17,1.,1.01883556321148E-16)) ;
#4761 = DIRECTION('ref_axis',(-1.,6.42891162084176E-17,-1.11022302462516E-16)) ;
#4762 = DIRECTION('',(1.,0.,-1.38524120452482E-15)) ;
#4763 = DIRECTION('',(-1.,0.,0.)) ;
#4764 = DIRECTION('center_axis',(6.42891162084177E-17,1.,1.01883556321148E-16)) ;
#4765 = DIRECTION('ref_axis',(-1.,6.42891162084177E-17,6.55000379205717E-33)) ;
#4766 = DIRECTION('center_axis',(0.0914655886839077,0.93797861604457,-0.334410170194956)) ;
#4767 = DIRECTION('ref_axis',(-0.225030533053291,0.346599923972543,0.910620531229106)) ;
#4768 = DIRECTION('center_axis',(0.226649657308027,0.937972680585475,-0.262368411432195)) ;
#4769 = DIRECTION('ref_axis',(-0.626757039824253,0.346652443702656,0.697859367140484)) ;
#4770 = DIRECTION('center_axis',(6.42891162084177E-17,1.,1.01883556321148E-16)) ;
#4771 = DIRECTION('ref_axis',(0.789438824149447,1.17867822247222E-17,-0.613829245739838)) ;
#4772 = DIRECTION('',(6.42891162084177E-17,1.,1.01883556321148E-16)) ;
#4773 = DIRECTION('center_axis',(6.42891162084177E-17,1.,1.01883556321148E-16)) ;
#4774 = DIRECTION('ref_axis',(-1.,6.42891162084177E-17,6.55000379205717E-33)) ;
#4775 = DIRECTION('',(6.42891162084177E-17,1.,1.01883556321148E-16)) ;
#4776 = DIRECTION('center_axis',(6.42891162084177E-17,1.,1.01883556321148E-16)) ;
#4777 = DIRECTION('ref_axis',(-1.,6.42891162084177E-17,6.55000379205717E-33)) ;
#4778 = DIRECTION('',(6.42891162084177E-17,1.,1.01883556321148E-16)) ;
#4779 = DIRECTION('center_axis',(-0.844327925302384,-3.10843368895129E-19,
0.535826795293564)) ;
#4780 = DIRECTION('ref_axis',(0.535826795293564,-1.20470962841276E-16,0.844327925302384)) ;
#4781 = DIRECTION('center_axis',(6.42891162084176E-17,1.,1.01883556321148E-16)) ;
#4782 = DIRECTION('ref_axis',(-1.,6.42891162084176E-17,-1.11022302462516E-16)) ;
#4783 = DIRECTION('center_axis',(6.42891162084177E-17,1.,1.01883556321148E-16)) ;
#4784 = DIRECTION('ref_axis',(-0.309016994374945,-7.70305906808054E-17,0.951056516295155)) ;
#4785 = DIRECTION('',(0.309016994374943,0.,-0.951056516295155)) ;
#4786 = DIRECTION('',(-0.309016994374945,0.,0.951056516295155)) ;
#4787 = DIRECTION('center_axis',(6.42891162084177E-17,1.,1.01883556321148E-16)) ;
#4788 = DIRECTION('ref_axis',(-0.309016994374945,-7.70305906808054E-17,0.951056516295154)) ;
#4789 = DIRECTION('center_axis',(-0.289778550198828,0.937978616044842,-0.190327369779724)) ;
#4790 = DIRECTION('ref_axis',(0.795750585755454,0.346611107728181,0.496630391004513)) ;
#4791 = DIRECTION('center_axis',(-0.179488590609232,0.937972680597995,-0.296632931908991)) ;
#4792 = DIRECTION('ref_axis',(0.462146062282483,0.346581069349003,0.816273593524682)) ;
#4793 = DIRECTION('center_axis',(6.42891162084177E-17,1.,1.01883556321148E-16)) ;
#4794 = DIRECTION('ref_axis',(-0.339836291371861,1.1766769120353E-16,-0.94048460650168)) ;
#4795 = DIRECTION('',(6.42891162084177E-17,1.,1.01883556321148E-16)) ;
#4796 = DIRECTION('center_axis',(6.42891162084177E-17,1.,1.01883556321148E-16)) ;
#4797 = DIRECTION('ref_axis',(-0.309016994374945,-7.70305906808053E-17,0.951056516295154)) ;
#4798 = DIRECTION('',(6.42891162084177E-17,1.,1.01883556321148E-16)) ;
#4799 = DIRECTION('center_axis',(6.42891162084177E-17,1.,1.01883556321148E-16)) ;
#4800 = DIRECTION('ref_axis',(-0.309016994374945,-7.70305906808054E-17,0.951056516295154)) ;
#4801 = DIRECTION('',(6.42891162084177E-17,1.,1.01883556321148E-16)) ;
#4802 = DIRECTION('center_axis',(0.248689887525719,-1.14670750118124E-16,
0.968583161035977)) ;
#4803 = DIRECTION('ref_axis',(0.968583161035977,-3.69319452351318E-17,-0.248689887525719)) ;
#4804 = DIRECTION('center_axis',(6.42891162084176E-17,1.,1.01883556321148E-16)) ;
#4805 = DIRECTION('ref_axis',(-1.,6.42891162084176E-17,-1.11022302462516E-16)) ;
#4806 = DIRECTION('center_axis',(6.42891162084176E-17,1.,1.01883556321148E-16)) ;
#4807 = DIRECTION('ref_axis',(0.809016994374951,-1.11896639422636E-16,0.587785252292469)) ;
#4808 = DIRECTION('',(-0.809016994374952,3.46310301131204E-16,-0.587785252292467)) ;
#4809 = DIRECTION('',(0.809016994374951,-3.67369352402517E-16,0.587785252292468)) ;
#4810 = DIRECTION('center_axis',(6.42891162084177E-17,1.,1.01883556321148E-16)) ;
#4811 = DIRECTION('ref_axis',(0.809016994374951,-1.11896639422636E-16,0.587785252292469)) ;
#4812 = DIRECTION('center_axis',(-0.270558581956355,0.937978616044069,0.216781386594465)) ;
#4813 = DIRECTION('ref_axis',(0.718062367667364,0.346609195532121,-0.603530033811504)) ;
#4814 = DIRECTION('center_axis',(-0.337579707503438,0.937972680589643,0.0790391773070337)) ;
#4815 = DIRECTION('ref_axis',(0.917158495892678,0.34665508108167,-0.196597426667139)) ;
#4816 = DIRECTION('center_axis',(6.42891162084177E-17,1.,1.01883556321148E-16)) ;
#4817 = DIRECTION('ref_axis',(-0.999469202827967,6.09358503167855E-17,0.0325777930257363)) ;
#4818 = DIRECTION('',(6.42891162084177E-17,1.,1.01883556321148E-16)) ;
#4819 = DIRECTION('center_axis',(6.42891162084177E-17,1.,1.01883556321148E-16)) ;
#4820 = DIRECTION('ref_axis',(0.809016994374951,-1.11896639422636E-16,0.587785252292469)) ;
#4821 = DIRECTION('',(6.42891162084177E-17,1.,1.01883556321148E-16)) ;
#4822 = DIRECTION('center_axis',(6.42891162084177E-17,1.,1.01883556321148E-16)) ;
#4823 = DIRECTION('ref_axis',(0.809016994374951,-1.11896639422636E-16,0.587785252292469)) ;
#4824 = DIRECTION('',(6.42891162084177E-17,1.,1.01883556321148E-16)) ;
#4825 = DIRECTION('center_axis',(0.998026728451666,-7.05595777195509E-17,
0.062790519157477)) ;
#4826 = DIRECTION('ref_axis',(0.062790519157477,9.76457654153146E-17,-0.998026728451666)) ;
#4827 = DIRECTION('center_axis',(6.42891162084176E-17,1.,1.01883556321148E-16)) ;
#4828 = DIRECTION('ref_axis',(0.809016994374942,7.8746642907257E-18,-0.58778525229248)) ;
#4829 = DIRECTION('',(-0.809016994374941,0.,0.587785252292482)) ;
#4830 = DIRECTION('',(0.809016994374942,0.,-0.58778525229248)) ;
#4831 = DIRECTION('center_axis',(6.42891162084177E-17,1.,1.01883556321148E-16)) ;
#4832 = DIRECTION('ref_axis',(0.809016994374942,7.87466429072562E-18,-0.58778525229248)) ;
#4833 = DIRECTION('center_axis',(0.122564151348405,0.937978616049674,0.324305634606899)) ;
#4834 = DIRECTION('ref_axis',(0.352942571631502,-0.346602105458515,0.869079122762632)) ;
#4835 = DIRECTION('center_axis',(-0.0291471407313505,0.937972680574302,0.345481829744264)) ;
#4836 = DIRECTION('ref_axis',(-0.10087517992079,-0.346624346328332,0.932564078553536)) ;
#4837 = DIRECTION('center_axis',(6.42891162084177E-17,1.,1.01883556321148E-16)) ;
#4838 = DIRECTION('ref_axis',(-0.27786964668458,-8.00072645743807E-17,0.960618789870043)) ;
#4839 = DIRECTION('',(6.42891162084177E-17,1.,1.01883556321148E-16)) ;
#4840 = DIRECTION('center_axis',(6.42891162084177E-17,1.,1.01883556321148E-16)) ;
#4841 = DIRECTION('ref_axis',(0.809016994374942,7.87466429072562E-18,-0.58778525229248)) ;
#4842 = DIRECTION('',(6.42891162084177E-17,1.,1.01883556321148E-16)) ;
#4843 = DIRECTION('center_axis',(6.42891162084177E-17,1.,1.01883556321148E-16)) ;
#4844 = DIRECTION('ref_axis',(0.809016994374942,7.87466429072562E-18,-0.58778525229248)) ;
#4845 = DIRECTION('',(6.42891162084177E-17,1.,1.01883556321148E-16)) ;
#4846 = DIRECTION('center_axis',(0.368124552338267,7.10625328556022E-17,-0.929776486025405)) ;
#4847 = DIRECTION('ref_axis',(-0.929776486025405,9.72803471192948E-17,-0.368124552338267)) ;
#4848 = DIRECTION('center_axis',(6.42891162084177E-17,1.,1.01883556321148E-16)) ;
#4849 = DIRECTION('ref_axis',(-0.309016994374958,1.16763449604299E-16,-0.95105651629515)) ;
#4850 = DIRECTION('',(0.30901699437496,-3.46310301131204E-16,0.95105651629515)) ;
#4851 = DIRECTION('',(-0.309016994374958,3.67369352402516E-16,-0.95105651629515)) ;
#4852 = DIRECTION('center_axis',(6.42891162084177E-17,1.,1.01883556321148E-16)) ;
#4853 = DIRECTION('ref_axis',(-0.309016994374958,1.16763449604299E-16,-0.95105651629515)) ;
#4854 = DIRECTION('center_axis',(0.346307392767925,0.93797861604615,-0.016349481778672)) ;
#4855 = DIRECTION('ref_axis',(0.935403580710108,-0.346577345830713,-0.0700305972532483)) ;
#4856 = DIRECTION('center_axis',(0.319565783679362,0.937972680572322,0.134480334626918)) ;
#4857 = DIRECTION('ref_axis',(0.856887437232556,-0.34664450139375,0.381551450746163)) ;
#4858 = DIRECTION('center_axis',(6.42891162084177E-17,1.,1.01883556321148E-16)) ;
#4859 = DIRECTION('ref_axis',(0.827736316734974,-1.10383059170658E-16,0.561117269345739)) ;
#4860 = DIRECTION('',(6.42891162084177E-17,1.,1.01883556321148E-16)) ;
#4861 = DIRECTION('center_axis',(6.42891162084177E-17,1.,1.01883556321148E-16)) ;
#4862 = DIRECTION('ref_axis',(-0.309016994374958,1.16763449604299E-16,-0.95105651629515)) ;
#4863 = DIRECTION('',(6.42891162084177E-17,1.,1.01883556321148E-16)) ;
#4864 = DIRECTION('center_axis',(6.42891162084177E-17,1.,1.01883556321148E-16)) ;
#4865 = DIRECTION('ref_axis',(-0.309016994374958,1.16763449604299E-16,-0.95105651629515)) ;
#4866 = DIRECTION('',(6.42891162084177E-17,1.,1.01883556321148E-16)) ;
#4867 = DIRECTION('center_axis',(-0.770513243013279,1.14478638350969E-16,
-0.637423989461614)) ;
#4868 = DIRECTION('ref_axis',(-0.637423989461614,-3.75232044582032E-17,0.770513243013279)) ;
#4869 = DIRECTION('axis',(0.,0.,1.)) ;
#4870 = DIRECTION('refdir',(1.,0.,0.)) ;
#4871 = DIRECTION('center_axis',(7.81669040162321E-17,1.,1.01883556321148E-16)) ;
#4872 = DIRECTION('ref_axis',(-1.,7.81669040162321E-17,-7.85614357465057E-33)) ;
#4873 = DIRECTION('center_axis',(-7.81669040162321E-17,-1.,-1.01883556321148E-16)) ;
#4874 = DIRECTION('ref_axis',(1.,-7.81669040162321E-17,7.85614357465057E-33)) ;
#4875 = DIRECTION('',(7.81669040162321E-17,1.,1.01883556321148E-16)) ;
#4876 = DIRECTION('center_axis',(-7.81669040162321E-17,-1.,-1.01883556321148E-16)) ;
#4877 = DIRECTION('ref_axis',(1.,-7.81669040162321E-17,-7.96392216778758E-33)) ;
#4878 = DIRECTION('center_axis',(7.81669040162321E-17,1.,1.01883556321148E-16)) ;
#4879 = DIRECTION('ref_axis',(-1.,7.81669040162321E-17,-7.79004302140918E-33)) ;
#4880 = DIRECTION('center_axis',(-7.81669040162321E-17,-1.,-1.01883556321148E-16)) ;
#4881 = DIRECTION('ref_axis',(1.,-7.81669040162321E-17,-7.96392216778758E-33)) ;
#4882 = DIRECTION('',(-7.81669040162321E-17,-1.,-1.01883556321148E-16)) ;
#4883 = DIRECTION('center_axis',(-7.81669040162321E-17,-1.,-1.01883556321148E-16)) ;
#4884 = DIRECTION('ref_axis',(1.,-7.81669040162321E-17,7.79004302140918E-33)) ;
#4885 = DIRECTION('center_axis',(-7.81669040162321E-17,-1.,-1.01883556321148E-16)) ;
#4886 = DIRECTION('ref_axis',(1.,-7.81669040162321E-17,1.11022302462516E-16)) ;
#4887 = DIRECTION('center_axis',(-7.81669040162321E-17,-1.,-1.01883556321148E-16)) ;
#4888 = DIRECTION('ref_axis',(1.,-7.81669040162321E-17,1.11022302462516E-16)) ;
#4889 = DIRECTION('axis',(0.,0.,1.)) ;
#4890 = DIRECTION('refdir',(1.,0.,0.)) ;
#4891 = DIRECTION('center_axis',(1.,4.03783642961741E-31,-1.15648231731787E-16)) ;
#4892 = DIRECTION('ref_axis',(1.15648231731787E-16,-3.49148133884313E-15,
1.)) ;
#4893 = DIRECTION('',(-1.15648231731787E-16,3.49148133884313E-15,-1.)) ;
#4894 = DIRECTION('',(0.,-1.,-3.49148133884313E-15)) ;
#4895 = DIRECTION('',(-1.15648231731787E-16,3.49148133884313E-15,-1.)) ;
#4896 = DIRECTION('',(0.,1.,3.49148133884313E-15)) ;
#4897 = DIRECTION('center_axis',(-1.73472347597681E-16,-3.49148133884313E-15,
1.)) ;
#4898 = DIRECTION('ref_axis',(-1.,6.05675464442612E-31,-1.73472347597681E-16)) ;
#4899 = DIRECTION('',(1.,-6.05675464442612E-31,1.73472347597681E-16)) ;
#4900 = DIRECTION('',(0.,-1.,-3.49148133884313E-15)) ;
#4901 = DIRECTION('',(1.,-6.05675464442612E-31,1.73472347597681E-16)) ;
#4902 = DIRECTION('',(0.,1.,3.49148133884313E-15)) ;
#4903 = DIRECTION('center_axis',(-1.,0.,0.)) ;
#4904 = DIRECTION('ref_axis',(0.,-1.,-3.49148133884313E-15)) ;
#4905 = DIRECTION('',(0.,-3.49148133884313E-15,1.)) ;
#4906 = DIRECTION('',(0.,1.,3.49148133884313E-15)) ;
#4907 = DIRECTION('',(0.,-3.49148133884313E-15,1.)) ;
#4908 = DIRECTION('',(0.,-1.,-3.49148133884313E-15)) ;
#4909 = DIRECTION('center_axis',(1.15648231731787E-16,3.49148133884313E-15,
-1.)) ;
#4910 = DIRECTION('ref_axis',(1.,-4.03783642961741E-31,1.15648231731787E-16)) ;
#4911 = DIRECTION('',(-1.,4.03783642961741E-31,-1.15648231731787E-16)) ;
#4912 = DIRECTION('',(0.,-1.,-3.49148133884313E-15)) ;
#4913 = DIRECTION('',(-1.,4.03783642961741E-31,-1.15648231731787E-16)) ;
#4914 = DIRECTION('',(0.,1.,3.49148133884313E-15)) ;
#4915 = DIRECTION('center_axis',(0.,-1.,-3.49148133884313E-15)) ;
#4916 = DIRECTION('ref_axis',(1.,0.,0.)) ;
#4917 = DIRECTION('center_axis',(0.,-1.,-3.49148133884313E-15)) ;
#4918 = DIRECTION('ref_axis',(1.,0.,0.)) ;
#4919 = DIRECTION('center_axis',(0.,-1.,-3.49148133884313E-15)) ;
#4920 = DIRECTION('ref_axis',(1.,0.,0.)) ;
#4921 = DIRECTION('center_axis',(0.,-1.,-3.49148133884313E-15)) ;
#4922 = DIRECTION('ref_axis',(1.,0.,0.)) ;
#4923 = DIRECTION('center_axis',(0.,-1.,-3.49148133884313E-15)) ;
#4924 = DIRECTION('ref_axis',(1.,0.,0.)) ;
#4925 = DIRECTION('center_axis',(0.,-1.,-3.49148133884313E-15)) ;
#4926 = DIRECTION('ref_axis',(1.,0.,0.)) ;
#4927 = DIRECTION('center_axis',(0.,1.,3.49148133884313E-15)) ;
#4928 = DIRECTION('ref_axis',(1.,0.,0.)) ;
#4929 = DIRECTION('center_axis',(0.,1.,3.49148133884313E-15)) ;
#4930 = DIRECTION('ref_axis',(1.,0.,0.)) ;
#4931 = DIRECTION('center_axis',(0.,1.,3.49148133884313E-15)) ;
#4932 = DIRECTION('ref_axis',(1.,0.,0.)) ;
#4933 = DIRECTION('center_axis',(0.,1.,3.49148133884313E-15)) ;
#4934 = DIRECTION('ref_axis',(1.,0.,0.)) ;
#4935 = DIRECTION('center_axis',(0.,1.,3.49148133884313E-15)) ;
#4936 = DIRECTION('ref_axis',(-1.,0.,0.)) ;
#4937 = DIRECTION('center_axis',(0.,1.,3.49148133884313E-15)) ;
#4938 = DIRECTION('ref_axis',(-1.,0.,0.)) ;
#4939 = DIRECTION('center_axis',(0.,1.,3.49148133884313E-15)) ;
#4940 = DIRECTION('ref_axis',(-1.,0.,0.)) ;
#4941 = DIRECTION('center_axis',(0.,1.,3.49148133884313E-15)) ;
#4942 = DIRECTION('ref_axis',(-1.,0.,0.)) ;
#4943 = DIRECTION('',(0.,0.,1.)) ;
#4944 = DIRECTION('',(1.,0.,0.)) ;
#4945 = DIRECTION('',(0.,0.,1.)) ;
#4946 = DIRECTION('',(1.,0.,0.)) ;
#4947 = DIRECTION('',(0.,0.,1.)) ;
#4948 = DIRECTION('',(1.,0.,0.)) ;
#4949 = DIRECTION('axis',(0.,0.,1.)) ;
#4950 = DIRECTION('refdir',(1.,0.,0.)) ;
#4951 = DIRECTION('axis',(0.,0.,1.)) ;
#4952 = DIRECTION('refdir',(1.,0.,0.)) ;
#4953 = DIRECTION('center_axis',(0.,-1.,-3.49148133884313E-15)) ;
#4954 = DIRECTION('ref_axis',(1.,0.,0.)) ;
#4955 = DIRECTION('center_axis',(0.,-1.,-3.49148133884313E-15)) ;
#4956 = DIRECTION('ref_axis',(1.,0.,0.)) ;
#4957 = DIRECTION('',(0.,-1.,-3.49148133884313E-15)) ;
#4958 = DIRECTION('center_axis',(0.,-1.,-3.49148133884313E-15)) ;
#4959 = DIRECTION('ref_axis',(1.,0.,0.)) ;
#4960 = DIRECTION('center_axis',(0.,-1.,-3.49148133884313E-15)) ;
#4961 = DIRECTION('ref_axis',(1.,0.,0.)) ;
#4962 = DIRECTION('',(0.,-3.49148133884313E-15,1.)) ;
#4963 = DIRECTION('',(-0.707106781186548,2.46885013108227E-15,-0.707106781186548)) ;
#4964 = DIRECTION('',(1.,-4.62017040814388E-31,1.32326939764619E-16)) ;
#4965 = DIRECTION('',(-0.707106781186548,-2.46885013108227E-15,0.707106781186548)) ;
#4966 = DIRECTION('',(0.,3.49148133884313E-15,-1.)) ;
#4967 = DIRECTION('',(0.707106781186547,-2.46885013108227E-15,0.707106781186547)) ;
#4968 = DIRECTION('',(-1.,4.62017040814388E-31,-1.32326939764619E-16)) ;
#4969 = DIRECTION('',(0.707106781186549,2.46885013108226E-15,-0.707106781186546)) ;
#4970 = DIRECTION('center_axis',(0.,-1.,-3.49148133884313E-15)) ;
#4971 = DIRECTION('ref_axis',(1.,0.,0.)) ;
#4972 = DIRECTION('',(1.,-4.62017040814388E-31,1.32326939764619E-16)) ;
#4973 = DIRECTION('',(0.707106781186548,-2.46885013108227E-15,0.707106781186548)) ;
#4974 = DIRECTION('',(0.,-3.49148133884313E-15,1.)) ;
#4975 = DIRECTION('',(-0.707106781186549,-2.46885013108226E-15,0.707106781186546)) ;
#4976 = DIRECTION('',(-1.,4.62017040814388E-31,-1.32326939764619E-16)) ;
#4977 = DIRECTION('',(-0.707106781186548,2.46885013108227E-15,-0.707106781186548)) ;
#4978 = DIRECTION('',(0.,3.49148133884313E-15,-1.)) ;
#4979 = DIRECTION('',(0.707106781186547,2.46885013108227E-15,-0.707106781186547)) ;
#4980 = DIRECTION('center_axis',(-0.707106781186548,-2.46885013108227E-15,
0.707106781186548)) ;
#4981 = DIRECTION('ref_axis',(3.82771347986811E-30,-1.,-3.49148133884313E-15)) ;
#4982 = DIRECTION('',(0.,1.,3.49148133884313E-15)) ;
#4983 = DIRECTION('',(0.,-1.,-3.49148133884313E-15)) ;
#4984 = DIRECTION('center_axis',(0.707106781186548,-2.46885013108227E-15,
0.707106781186548)) ;
#4985 = DIRECTION('ref_axis',(-3.82771347986811E-30,-1.,-3.49148133884313E-15)) ;
#4986 = DIRECTION('',(0.,1.,3.49148133884313E-15)) ;
#4987 = DIRECTION('',(0.,-1.,-3.49148133884313E-15)) ;
#4988 = DIRECTION('center_axis',(0.707106781186548,2.46885013108227E-15,-0.707106781186548)) ;
#4989 = DIRECTION('ref_axis',(3.82771347986811E-30,-1.,-3.49148133884313E-15)) ;
#4990 = DIRECTION('',(0.,1.,3.49148133884313E-15)) ;
#4991 = DIRECTION('',(0.,-1.,-3.49148133884313E-15)) ;
#4992 = DIRECTION('center_axis',(-0.707106781186546,2.46885013108227E-15,
-0.707106781186549)) ;
#4993 = DIRECTION('ref_axis',(-1.32640682077634E-30,-1.,-3.49148133884313E-15)) ;
#4994 = DIRECTION('',(0.,1.,3.49148133884313E-15)) ;
#4995 = DIRECTION('',(0.,-1.,-3.49148133884313E-15)) ;
#4996 = DIRECTION('center_axis',(-1.,0.,0.)) ;
#4997 = DIRECTION('ref_axis',(0.,-1.,-3.49148133884313E-15)) ;
#4998 = DIRECTION('',(-1.38951567537567E-16,-5.77315972805081E-15,1.)) ;
#4999 = DIRECTION('center_axis',(-1.,0.,0.)) ;
#5000 = DIRECTION('ref_axis',(0.,1.,0.)) ;
#5001 = DIRECTION('center_axis',(-1.,0.,0.)) ;
#5002 = DIRECTION('ref_axis',(0.,1.,0.)) ;
#5003 = DIRECTION('center_axis',(-1.,0.,0.)) ;
#5004 = DIRECTION('ref_axis',(0.,-1.,-3.49148133884313E-15)) ;
#5005 = DIRECTION('center_axis',(1.,0.,0.)) ;
#5006 = DIRECTION('ref_axis',(0.,1.,0.)) ;
#5007 = DIRECTION('',(-1.38951567537567E-16,-5.77315972805081E-15,1.)) ;
#5008 = DIRECTION('center_axis',(1.,0.,0.)) ;
#5009 = DIRECTION('ref_axis',(0.,1.,0.)) ;
#5010 = DIRECTION('center_axis',(1.,0.,0.)) ;
#5011 = DIRECTION('ref_axis',(0.,-1.00929365875017E-14,1.)) ;
#5012 = DIRECTION('',(-1.,4.85146805060415E-31,-1.38951567537567E-16)) ;
#5013 = DIRECTION('center_axis',(1.,0.,0.)) ;
#5014 = DIRECTION('ref_axis',(0.,0.,1.)) ;
#5015 = DIRECTION('',(1.,-4.85146805060415E-31,1.38951567537567E-16)) ;
#5016 = DIRECTION('center_axis',(-1.,8.13374953119913E-31,-1.38951567537567E-16)) ;
#5017 = DIRECTION('ref_axis',(1.38951567537567E-16,3.49148133884313E-15,-1.)) ;
#5018 = DIRECTION('',(4.37905770101505E-47,1.,5.85365798698176E-15)) ;
#5019 = DIRECTION('',(1.38951567537567E-16,6.98296267768627E-15,-1.)) ;
#5020 = DIRECTION('',(4.37905770101505E-47,1.,5.85365798698176E-15)) ;
#5021 = DIRECTION('center_axis',(1.,-8.13374953119913E-31,1.38951567537567E-16)) ;
#5022 = DIRECTION('ref_axis',(-1.38951567537567E-16,-3.49148133884313E-15,
1.)) ;
#5023 = DIRECTION('',(-4.37905770101505E-47,-1.,-5.85365798698176E-15)) ;
#5024 = DIRECTION('',(1.38951567537567E-16,6.98296267768627E-15,-1.)) ;
#5025 = DIRECTION('',(-4.37905770101505E-47,-1.,-5.85365798698176E-15)) ;
#5026 = DIRECTION('center_axis',(1.38951567537567E-16,5.85365798698176E-15,
-1.)) ;
#5027 = DIRECTION('ref_axis',(0.,1.,5.85365798698176E-15)) ;
#5028 = DIRECTION('',(-1.,4.85146805060415E-31,-1.38951567537567E-16)) ;
#5029 = DIRECTION('center_axis',(1.38951567537567E-16,5.85365798698176E-15,
-1.)) ;
#5030 = DIRECTION('ref_axis',(0.,1.,5.85365798698176E-15)) ;
#5031 = DIRECTION('',(-1.,4.85146805060415E-31,-1.38951567537567E-16)) ;
#5032 = DIRECTION('center_axis',(4.85146805060415E-31,-1.,-6.98296267768627E-15)) ;
#5033 = DIRECTION('ref_axis',(1.36633227546431E-61,6.98296267768627E-15,-1.)) ;
#5034 = DIRECTION('center_axis',(0.,-3.38306112159458E-15,1.)) ;
#5035 = DIRECTION('ref_axis',(0.,-1.,-3.38306112159458E-15)) ;
#5036 = DIRECTION('',(1.,-2.28167838920768E-15,-7.96643751716028E-30)) ;
#5037 = DIRECTION('center_axis',(0.,-3.38306112159458E-15,1.)) ;
#5038 = DIRECTION('ref_axis',(0.,1.,3.38306112159458E-15)) ;
#5039 = DIRECTION('center_axis',(0.,-3.38306112159458E-15,1.)) ;
#5040 = DIRECTION('ref_axis',(0.,1.,3.38306112159458E-15)) ;
#5041 = DIRECTION('center_axis',(0.,-3.38306112159458E-15,1.)) ;
#5042 = DIRECTION('ref_axis',(0.,-1.,-3.38306112159458E-15)) ;
#5043 = DIRECTION('center_axis',(0.,3.38306112159458E-15,-1.)) ;
#5044 = DIRECTION('ref_axis',(0.,1.,3.38306112159458E-15)) ;
#5045 = DIRECTION('',(1.,-2.28167838920768E-15,-7.96643751716028E-30)) ;
#5046 = DIRECTION('center_axis',(0.,3.38306112159458E-15,-1.)) ;
#5047 = DIRECTION('ref_axis',(0.,1.,3.38306112159458E-15)) ;
#5048 = DIRECTION('center_axis',(0.,3.38306112159458E-15,-1.)) ;
#5049 = DIRECTION('ref_axis',(1.,0.,0.)) ;
#5050 = DIRECTION('',(1.64114074029749E-31,-3.42200555507435E-15,1.)) ;
#5051 = DIRECTION('center_axis',(0.,3.38306112159458E-15,-1.)) ;
#5052 = DIRECTION('ref_axis',(1.,0.,0.)) ;
#5053 = DIRECTION('',(-1.64114074029749E-31,3.42200555507435E-15,-1.)) ;
#5054 = DIRECTION('center_axis',(0.,-3.49148133884313E-15,1.)) ;
#5055 = DIRECTION('ref_axis',(0.,-1.,-3.49148133884313E-15)) ;
#5056 = DIRECTION('',(2.36217664813863E-15,1.,3.49148133884313E-15)) ;
#5057 = DIRECTION('',(-1.,3.49148133884313E-15,1.21904419394898E-29)) ;
#5058 = DIRECTION('',(2.36217664813863E-15,1.,3.49148133884313E-15)) ;
#5059 = DIRECTION('center_axis',(0.,3.49148133884313E-15,-1.)) ;
#5060 = DIRECTION('ref_axis',(0.,1.,3.49148133884313E-15)) ;
#5061 = DIRECTION('',(-2.36217664813863E-15,-1.,-3.49148133884313E-15)) ;
#5062 = DIRECTION('',(-1.,3.49148133884313E-15,1.21904419394898E-29)) ;
#5063 = DIRECTION('',(-2.36217664813863E-15,-1.,-3.49148133884313E-15)) ;
#5064 = DIRECTION('center_axis',(-1.,2.36217664813863E-15,8.24749568602705E-30)) ;
#5065 = DIRECTION('ref_axis',(-2.36217664813863E-15,-1.,-3.49148133884313E-15)) ;
#5066 = DIRECTION('',(0.,-3.49148133884313E-15,1.)) ;
#5067 = DIRECTION('center_axis',(-1.,2.36217664813863E-15,8.24749568602705E-30)) ;
#5068 = DIRECTION('ref_axis',(-2.36217664813863E-15,-1.,-3.49148133884313E-15)) ;
#5069 = DIRECTION('',(0.,-3.49148133884313E-15,1.)) ;
#5070 = DIRECTION('center_axis',(-3.49148133884313E-15,-1.,-3.49148133884313E-15)) ;
#5071 = DIRECTION('ref_axis',(1.,-3.49148133884313E-15,-1.21904419394898E-29)) ;
#5072 = DIRECTION('center_axis',(1.,0.,0.)) ;
#5073 = DIRECTION('ref_axis',(0.,1.,3.49148133884313E-15)) ;
#5074 = DIRECTION('',(1.38951567537567E-16,1.20980294963545E-15,-1.)) ;
#5075 = DIRECTION('center_axis',(1.,0.,0.)) ;
#5076 = DIRECTION('ref_axis',(0.,-1.,-1.38777878078146E-14)) ;
#5077 = DIRECTION('center_axis',(1.,0.,0.)) ;
#5078 = DIRECTION('ref_axis',(0.,-1.,-1.00929365875015E-14)) ;
#5079 = DIRECTION('center_axis',(1.,0.,0.)) ;
#5080 = DIRECTION('ref_axis',(0.,1.,3.49148133884313E-15)) ;
#5081 = DIRECTION('center_axis',(-1.,0.,0.)) ;
#5082 = DIRECTION('ref_axis',(0.,-1.,0.)) ;
#5083 = DIRECTION('',(1.38951567537567E-16,1.20980294963545E-15,-1.)) ;
#5084 = DIRECTION('center_axis',(-1.,0.,0.)) ;
#5085 = DIRECTION('ref_axis',(0.,-1.,0.)) ;
#5086 = DIRECTION('center_axis',(-1.,0.,0.)) ;
#5087 = DIRECTION('ref_axis',(0.,0.,-1.)) ;
#5088 = DIRECTION('',(1.,-4.85146805060415E-31,1.38951567537567E-16)) ;
#5089 = DIRECTION('center_axis',(-1.,0.,0.)) ;
#5090 = DIRECTION('ref_axis',(0.,0.,-1.)) ;
#5091 = DIRECTION('',(-1.,4.85146805060415E-31,-1.38951567537567E-16)) ;
#5092 = DIRECTION('center_axis',(1.,-1.56918657000917E-31,1.38951567537567E-16)) ;
#5093 = DIRECTION('ref_axis',(-1.38951567537567E-16,-3.49148133884313E-15,
1.)) ;
#5094 = DIRECTION('',(0.,1.,1.1293046907045E-15)) ;
#5095 = DIRECTION('',(-1.38951567537567E-16,0.,1.)) ;
#5096 = DIRECTION('',(0.,1.,1.1293046907045E-15)) ;
#5097 = DIRECTION('center_axis',(-1.,1.56918657000917E-31,-1.38951567537567E-16)) ;
#5098 = DIRECTION('ref_axis',(1.38951567537567E-16,3.49148133884313E-15,-1.)) ;
#5099 = DIRECTION('',(0.,-1.,-1.1293046907045E-15)) ;
#5100 = DIRECTION('',(-1.38951567537567E-16,0.,1.)) ;
#5101 = DIRECTION('',(0.,-1.,-1.1293046907045E-15)) ;
#5102 = DIRECTION('center_axis',(-1.38951567537567E-16,-1.1293046907045E-15,
1.)) ;
#5103 = DIRECTION('ref_axis',(0.,-1.,-1.1293046907045E-15)) ;
#5104 = DIRECTION('',(1.,-4.85146805060415E-31,1.38951567537567E-16)) ;
#5105 = DIRECTION('center_axis',(-1.38951567537567E-16,-1.1293046907045E-15,
1.)) ;
#5106 = DIRECTION('ref_axis',(0.,-1.,-1.1293046907045E-15)) ;
#5107 = DIRECTION('',(1.,-4.85146805060415E-31,1.38951567537567E-16)) ;
#5108 = DIRECTION('center_axis',(-4.85146805060415E-31,-1.,0.)) ;
#5109 = DIRECTION('ref_axis',(0.,0.,-1.)) ;
#5110 = DIRECTION('center_axis',(0.,3.49148133884313E-15,-1.)) ;
#5111 = DIRECTION('ref_axis',(0.,1.,3.49148133884313E-15)) ;
#5112 = DIRECTION('',(-1.,-2.28167838920768E-15,-7.96643751716028E-30)) ;
#5113 = DIRECTION('center_axis',(0.,3.49148133884313E-15,-1.)) ;
#5114 = DIRECTION('ref_axis',(0.,-1.,-3.49148133884313E-15)) ;
#5115 = DIRECTION('center_axis',(0.,3.49148133884313E-15,-1.)) ;
#5116 = DIRECTION('ref_axis',(0.,-1.,-3.49148133884313E-15)) ;
#5117 = DIRECTION('center_axis',(0.,3.49148133884313E-15,-1.)) ;
#5118 = DIRECTION('ref_axis',(0.,1.,3.49148133884313E-15)) ;
#5119 = DIRECTION('center_axis',(0.,-3.49148133884313E-15,1.)) ;
#5120 = DIRECTION('ref_axis',(0.,-1.,-3.49148133884313E-15)) ;
#5121 = DIRECTION('',(-1.,-2.28167838920768E-15,-7.96643751716028E-30)) ;
#5122 = DIRECTION('center_axis',(0.,-3.49148133884313E-15,1.)) ;
#5123 = DIRECTION('ref_axis',(0.,-1.,-3.49148133884313E-15)) ;
#5124 = DIRECTION('center_axis',(0.,-3.49148133884313E-15,1.)) ;
#5125 = DIRECTION('ref_axis',(-1.,0.,0.)) ;
#5126 = DIRECTION('',(0.,3.49148133884313E-15,-1.)) ;
#5127 = DIRECTION('center_axis',(0.,-3.49148133884313E-15,1.)) ;
#5128 = DIRECTION('ref_axis',(-1.,0.,0.)) ;
#5129 = DIRECTION('',(0.,-3.49148133884313E-15,1.)) ;
#5130 = DIRECTION('center_axis',(0.,3.49148133884313E-15,-1.)) ;
#5131 = DIRECTION('ref_axis',(0.,1.,3.49148133884313E-15)) ;
#5132 = DIRECTION('',(-2.36217664813863E-15,1.,3.49148133884313E-15)) ;
#5133 = DIRECTION('',(1.,3.49148133884313E-15,1.21904419394898E-29)) ;
#5134 = DIRECTION('',(-2.36217664813863E-15,1.,3.49148133884313E-15)) ;
#5135 = DIRECTION('center_axis',(0.,-3.49148133884313E-15,1.)) ;
#5136 = DIRECTION('ref_axis',(0.,-1.,-3.49148133884313E-15)) ;
#5137 = DIRECTION('',(2.36217664813863E-15,-1.,-3.49148133884313E-15)) ;
#5138 = DIRECTION('',(1.,3.49148133884313E-15,1.21904419394898E-29)) ;
#5139 = DIRECTION('',(2.36217664813863E-15,-1.,-3.49148133884313E-15)) ;
#5140 = DIRECTION('center_axis',(1.,2.36217664813863E-15,8.24749568602705E-30)) ;
#5141 = DIRECTION('ref_axis',(-2.36217664813863E-15,1.,3.49148133884313E-15)) ;
#5142 = DIRECTION('',(0.,3.49148133884313E-15,-1.)) ;
#5143 = DIRECTION('center_axis',(1.,2.36217664813863E-15,8.24749568602705E-30)) ;
#5144 = DIRECTION('ref_axis',(-2.36217664813863E-15,1.,3.49148133884313E-15)) ;
#5145 = DIRECTION('',(0.,3.49148133884313E-15,-1.)) ;
#5146 = DIRECTION('center_axis',(3.49148133884313E-15,-1.,-3.49148133884313E-15)) ;
#5147 = DIRECTION('ref_axis',(1.,3.49148133884313E-15,1.21904419394898E-29)) ;
#5148 = DIRECTION('axis',(0.,0.,1.)) ;
#5149 = DIRECTION('refdir',(1.,0.,0.)) ;
#5150 = DIRECTION('center_axis',(1.02015335365891E-16,0.,1.)) ;
#5151 = DIRECTION('ref_axis',(-1.,0.,0.)) ;
#5152 = DIRECTION('center_axis',(-1.,0.,1.02015335365891E-16)) ;
#5153 = DIRECTION('ref_axis',(1.02015335365891E-16,0.,1.)) ;
#5154 = DIRECTION('center_axis',(-1.02015335365891E-16,0.,-1.)) ;
#5155 = DIRECTION('ref_axis',(-1.,0.,1.02015335365891E-16)) ;
#5156 = DIRECTION('center_axis',(0.,1.,0.)) ;
#5157 = DIRECTION('ref_axis',(0.,0.,1.)) ;
#5158 = DIRECTION('center_axis',(0.,1.,0.)) ;
#5159 = DIRECTION('ref_axis',(0.,0.,1.)) ;
#5160 = DIRECTION('center_axis',(1.02015335365891E-16,0.,1.)) ;
#5161 = DIRECTION('ref_axis',(-1.,0.,0.)) ;
#5162 = DIRECTION('center_axis',(-0.93947030108257,-0.342630345100702,9.58403778312327E-17)) ;
#5163 = DIRECTION('ref_axis',(9.00391886169754E-17,3.28378217308969E-17,1.)) ;
#5164 = DIRECTION('center_axis',(-1.02015335365891E-16,0.,-1.)) ;
#5165 = DIRECTION('ref_axis',(-1.,0.,1.02015335365891E-16)) ;
#5166 = DIRECTION('center_axis',(-1.,0.,1.02015335365891E-16)) ;
#5167 = DIRECTION('ref_axis',(1.02015335365891E-16,0.,1.)) ;
#5168 = DIRECTION('center_axis',(-1.02015335365891E-16,0.,-1.)) ;
#5169 = DIRECTION('ref_axis',(1.,0.,0.)) ;
#5170 = DIRECTION('center_axis',(-1.,0.,1.02015335365891E-16)) ;
#5171 = DIRECTION('ref_axis',(1.02015335365891E-16,0.,1.)) ;
#5172 = DIRECTION('center_axis',(-1.,0.,1.02015335365891E-16)) ;
#5173 = DIRECTION('ref_axis',(1.02015335365891E-16,0.,1.)) ;
#5174 = DIRECTION('center_axis',(1.02015335365891E-16,0.,1.)) ;
#5175 = DIRECTION('ref_axis',(1.,0.,-1.02015335365891E-16)) ;
#5176 = DIRECTION('center_axis',(-0.93947030108257,-0.342630345100702,9.58403778312327E-17)) ;
#5177 = DIRECTION('ref_axis',(9.00391886169754E-17,3.28378217308969E-17,1.)) ;
#5178 = DIRECTION('center_axis',(-0.93947030108257,-0.342630345100702,9.58403778312327E-17)) ;
#5179 = DIRECTION('ref_axis',(9.00391886169754E-17,3.28378217308969E-17,1.)) ;
#5180 = DIRECTION('center_axis',(0.,-1.,0.)) ;
#5181 = DIRECTION('ref_axis',(0.,0.,-1.)) ;
#5182 = DIRECTION('center_axis',(-1.,0.,1.02015335365891E-16)) ;
#5183 = DIRECTION('ref_axis',(1.02015335365891E-16,0.,1.)) ;
#5184 = DIRECTION('center_axis',(0.,1.,0.)) ;
#5185 = DIRECTION('ref_axis',(0.,0.,-1.)) ;
#5186 = DIRECTION('center_axis',(1.,0.,0.)) ;
#5187 = DIRECTION('ref_axis',(0.,0.,-1.)) ;
#5188 = DIRECTION('center_axis',(1.,0.,0.)) ;
#5189 = DIRECTION('ref_axis',(0.,0.,-1.)) ;
#5190 = DIRECTION('center_axis',(-1.,0.,1.02015335365891E-16)) ;
#5191 = DIRECTION('ref_axis',(1.02015335365891E-16,0.,1.)) ;
#5192 = DIRECTION('center_axis',(1.,0.,0.)) ;
#5193 = DIRECTION('ref_axis',(0.,0.,-1.)) ;
#5194 = DIRECTION('center_axis',(0.,1.,0.)) ;
#5195 = DIRECTION('ref_axis',(0.,0.,1.)) ;
#5196 = DIRECTION('center_axis',(0.,1.,0.)) ;
#5197 = DIRECTION('ref_axis',(0.,0.,1.)) ;
#5198 = DIRECTION('center_axis',(-1.,0.,0.)) ;
#5199 = DIRECTION('ref_axis',(0.,0.,-1.)) ;
#5200 = DIRECTION('center_axis',(0.,-1.,0.)) ;
#5201 = DIRECTION('ref_axis',(0.,0.,-1.)) ;
#5202 = DIRECTION('center_axis',(0.,-1.,0.)) ;
#5203 = DIRECTION('ref_axis',(0.,0.,-1.)) ;
#5204 = DIRECTION('center_axis',(0.,0.,-1.)) ;
#5205 = DIRECTION('ref_axis',(-1.,0.,0.)) ;
#5206 = DIRECTION('center_axis',(0.,-1.,0.)) ;
#5207 = DIRECTION('ref_axis',(0.,0.,-1.)) ;
#5208 = DIRECTION('center_axis',(0.,-1.,0.)) ;
#5209 = DIRECTION('ref_axis',(0.,0.,-1.)) ;
#5210 = DIRECTION('center_axis',(0.,0.,1.)) ;
#5211 = DIRECTION('ref_axis',(-1.,0.,0.)) ;
#5212 = DIRECTION('center_axis',(1.,0.,0.)) ;
#5213 = DIRECTION('ref_axis',(0.,0.,-1.)) ;
#5214 = DIRECTION('center_axis',(0.,0.,-1.)) ;
#5215 = DIRECTION('ref_axis',(-1.,0.,0.)) ;
#5216 = DIRECTION('center_axis',(1.,0.,0.)) ;
#5217 = DIRECTION('ref_axis',(0.,0.,-1.)) ;
#5218 = DIRECTION('center_axis',(0.,0.,1.)) ;
#5219 = DIRECTION('ref_axis',(-1.,0.,0.)) ;
#5220 = DIRECTION('center_axis',(0.93947030108257,0.342630345100702,0.)) ;
#5221 = DIRECTION('ref_axis',(0.,0.,-1.)) ;
#5222 = DIRECTION('center_axis',(0.,0.,1.)) ;
#5223 = DIRECTION('ref_axis',(1.,0.,0.)) ;
#5224 = DIRECTION('center_axis',(0.93947030108257,0.342630345100702,0.)) ;
#5225 = DIRECTION('ref_axis',(0.,0.,-1.)) ;
#5226 = DIRECTION('center_axis',(0.93947030108257,0.342630345100702,0.)) ;
#5227 = DIRECTION('ref_axis',(0.,0.,-1.)) ;
#5228 = DIRECTION('center_axis',(0.,0.,-1.)) ;
#5229 = DIRECTION('ref_axis',(1.,0.,0.)) ;
#5230 = DIRECTION('center_axis',(1.,0.,0.)) ;
#5231 = DIRECTION('ref_axis',(0.,0.,-1.)) ;
#5232 = DIRECTION('center_axis',(1.,0.,0.)) ;
#5233 = DIRECTION('ref_axis',(0.,0.,-1.)) ;
#5234 = DIRECTION('center_axis',(0.,-1.,0.)) ;
#5235 = DIRECTION('ref_axis',(0.,0.,1.)) ;
#5236 = DIRECTION('',(0.,1.,0.)) ;
#5237 = DIRECTION('center_axis',(1.,1.91189112624469E-17,-1.02015335365891E-16)) ;
#5238 = DIRECTION('ref_axis',(-1.91189112624469E-17,1.,1.95042214426922E-33)) ;
#5239 = DIRECTION('',(-1.,-1.91189112624469E-17,1.02015335365891E-16)) ;
#5240 = DIRECTION('center_axis',(0.93947030108257,0.342630345100702,-9.58403778312327E-17)) ;
#5241 = DIRECTION('ref_axis',(-0.342630345100702,0.93947030108257,3.97141584069169E-32)) ;
#5242 = DIRECTION('',(-0.93947030108257,-0.342630345100702,9.58403778312327E-17)) ;
#5243 = DIRECTION('center_axis',(1.,0.,-1.02015335365891E-16)) ;
#5244 = DIRECTION('ref_axis',(1.02015335365891E-16,0.,1.)) ;
#5245 = DIRECTION('',(-1.,0.,1.02015335365891E-16)) ;
#5246 = DIRECTION('center_axis',(0.,-1.,0.)) ;
#5247 = DIRECTION('ref_axis',(0.,0.,-1.)) ;
#5248 = DIRECTION('',(0.,1.,0.)) ;
#5249 = DIRECTION('center_axis',(1.,1.91189112624469E-17,0.)) ;
#5250 = DIRECTION('ref_axis',(-1.91189112624469E-17,1.,0.)) ;
#5251 = DIRECTION('',(-1.,-1.91189112624469E-17,0.)) ;
#5252 = DIRECTION('center_axis',(0.93947030108257,0.342630345100702,0.)) ;
#5253 = DIRECTION('ref_axis',(-0.342630345100702,0.93947030108257,0.)) ;
#5254 = DIRECTION('',(-0.93947030108257,-0.342630345100702,0.)) ;
#5255 = DIRECTION('center_axis',(1.,0.,0.)) ;
#5256 = DIRECTION('ref_axis',(0.,0.,-1.)) ;
#5257 = DIRECTION('',(-1.,0.,0.)) ;
#5258 = DIRECTION('axis',(0.,0.,1.)) ;
#5259 = DIRECTION('refdir',(1.,0.,0.)) ;
#5260 = DIRECTION('center_axis',(-1.,0.,-3.38946600347724E-15)) ;
#5261 = DIRECTION('ref_axis',(3.38353683695287E-15,0.,-1.)) ;
#5262 = DIRECTION('center_axis',(3.38946600347724E-15,0.,-1.)) ;
#5263 = DIRECTION('ref_axis',(-1.,0.,-3.38946600347724E-15)) ;
#5264 = DIRECTION('center_axis',(1.,0.,3.38946600347724E-15)) ;
#5265 = DIRECTION('ref_axis',(3.38946600347724E-15,0.,-1.)) ;
#5266 = DIRECTION('center_axis',(0.,1.,0.)) ;
#5267 = DIRECTION('ref_axis',(-1.,0.,0.)) ;
#5268 = DIRECTION('center_axis',(0.,1.,0.)) ;
#5269 = DIRECTION('ref_axis',(-1.,0.,0.)) ;
#5270 = DIRECTION('center_axis',(-1.,0.,-3.38946600347724E-15)) ;
#5271 = DIRECTION('ref_axis',(4.09928501400059E-15,0.,-1.)) ;
#5272 = DIRECTION('center_axis',(3.1843026467959E-15,-0.342630345100702,-0.93947030108257)) ;
#5273 = DIRECTION('ref_axis',(-1.,-1.09103871477676E-15,-2.99155776632337E-15)) ;
#5274 = DIRECTION('center_axis',(1.,0.,3.38946600347724E-15)) ;
#5275 = DIRECTION('ref_axis',(3.38946600347724E-15,0.,-1.)) ;
#5276 = DIRECTION('center_axis',(3.38946600347724E-15,0.,-1.)) ;
#5277 = DIRECTION('ref_axis',(-1.,0.,-3.38946600347724E-15)) ;
#5278 = DIRECTION('center_axis',(1.,0.,3.38946600347724E-15)) ;
#5279 = DIRECTION('ref_axis',(-4.09928501400059E-15,0.,1.)) ;
#5280 = DIRECTION('center_axis',(3.38946600347724E-15,0.,-1.)) ;
#5281 = DIRECTION('ref_axis',(-1.,0.,-3.38946600347724E-15)) ;
#5282 = DIRECTION('center_axis',(3.38946600347724E-15,0.,-1.)) ;
#5283 = DIRECTION('ref_axis',(-1.,0.,-3.38946600347724E-15)) ;
#5284 = DIRECTION('center_axis',(-1.,0.,-3.38946600347724E-15)) ;
#5285 = DIRECTION('ref_axis',(-3.38946600347724E-15,0.,1.)) ;
#5286 = DIRECTION('center_axis',(3.1843026467959E-15,-0.342630345100702,-0.93947030108257)) ;
#5287 = DIRECTION('ref_axis',(-1.,-1.09103871477676E-15,-2.99155776632337E-15)) ;
#5288 = DIRECTION('center_axis',(3.1843026467959E-15,-0.342630345100702,-0.93947030108257)) ;
#5289 = DIRECTION('ref_axis',(-1.,-1.09103871477676E-15,-2.99155776632337E-15)) ;
#5290 = DIRECTION('center_axis',(0.,-1.,0.)) ;
#5291 = DIRECTION('ref_axis',(1.,0.,0.)) ;
#5292 = DIRECTION('center_axis',(3.38946600347724E-15,0.,-1.)) ;
#5293 = DIRECTION('ref_axis',(-1.,0.,-3.38946600347724E-15)) ;
#5294 = DIRECTION('center_axis',(0.,1.,0.)) ;
#5295 = DIRECTION('ref_axis',(1.,0.,0.)) ;
#5296 = DIRECTION('center_axis',(-3.49148133884313E-15,0.,1.)) ;
#5297 = DIRECTION('ref_axis',(1.,0.,3.49148133884313E-15)) ;
#5298 = DIRECTION('center_axis',(-3.49148133884313E-15,0.,1.)) ;
#5299 = DIRECTION('ref_axis',(1.,0.,3.49148133884313E-15)) ;
#5300 = DIRECTION('center_axis',(3.38946600347724E-15,0.,-1.)) ;
#5301 = DIRECTION('ref_axis',(-1.,0.,-3.38946600347724E-15)) ;
#5302 = DIRECTION('center_axis',(-3.49148133884313E-15,0.,1.)) ;
#5303 = DIRECTION('ref_axis',(1.,0.,0.)) ;
#5304 = DIRECTION('center_axis',(0.,1.,0.)) ;
#5305 = DIRECTION('ref_axis',(-1.,0.,0.)) ;
#5306 = DIRECTION('center_axis',(0.,1.,0.)) ;
#5307 = DIRECTION('ref_axis',(-1.,0.,0.)) ;
#5308 = DIRECTION('center_axis',(3.49148133884313E-15,0.,-1.)) ;
#5309 = DIRECTION('ref_axis',(1.,0.,3.49148133884313E-15)) ;
#5310 = DIRECTION('center_axis',(0.,-1.,0.)) ;
#5311 = DIRECTION('ref_axis',(1.,0.,0.)) ;
#5312 = DIRECTION('center_axis',(0.,-1.,0.)) ;
#5313 = DIRECTION('ref_axis',(1.,0.,0.)) ;
#5314 = DIRECTION('center_axis',(1.,0.,3.49148133884313E-15)) ;
#5315 = DIRECTION('ref_axis',(3.38353683695287E-15,0.,-1.)) ;
#5316 = DIRECTION('center_axis',(0.,-1.,0.)) ;
#5317 = DIRECTION('ref_axis',(1.,0.,0.)) ;
#5318 = DIRECTION('center_axis',(0.,-1.,0.)) ;
#5319 = DIRECTION('ref_axis',(1.,0.,0.)) ;
#5320 = DIRECTION('center_axis',(-1.,0.,-3.49148133884313E-15)) ;
#5321 = DIRECTION('ref_axis',(3.49148133884313E-15,0.,-1.)) ;
#5322 = DIRECTION('center_axis',(-3.49148133884313E-15,0.,1.)) ;
#5323 = DIRECTION('ref_axis',(1.,0.,3.49148133884313E-15)) ;
#5324 = DIRECTION('center_axis',(1.,0.,3.49148133884313E-15)) ;
#5325 = DIRECTION('ref_axis',(4.09928501400059E-15,0.,-1.)) ;
#5326 = DIRECTION('center_axis',(-3.49148133884313E-15,0.,1.)) ;
#5327 = DIRECTION('ref_axis',(1.,0.,3.49148133884313E-15)) ;
#5328 = DIRECTION('center_axis',(-1.,0.,-3.49148133884313E-15)) ;
#5329 = DIRECTION('ref_axis',(3.49148133884313E-15,0.,-1.)) ;
#5330 = DIRECTION('center_axis',(-3.28014302462713E-15,0.342630345100702,
0.93947030108257)) ;
#5331 = DIRECTION('ref_axis',(1.,1.12387653650765E-15,3.08159695494034E-15)) ;
#5332 = DIRECTION('center_axis',(-1.,0.,-3.49148133884313E-15)) ;
#5333 = DIRECTION('ref_axis',(-4.09928501400059E-15,0.,1.)) ;
#5334 = DIRECTION('center_axis',(-3.28014302462713E-15,0.342630345100702,
0.93947030108257)) ;
#5335 = DIRECTION('ref_axis',(1.,1.12387653650765E-15,3.08159695494034E-15)) ;
#5336 = DIRECTION('center_axis',(-3.28014302462713E-15,0.342630345100702,
0.93947030108257)) ;
#5337 = DIRECTION('ref_axis',(1.,1.12387653650765E-15,3.08159695494034E-15)) ;
#5338 = DIRECTION('center_axis',(1.,0.,3.49148133884313E-15)) ;
#5339 = DIRECTION('ref_axis',(-3.49148133884313E-15,0.,1.)) ;
#5340 = DIRECTION('center_axis',(-3.49148133884313E-15,0.,1.)) ;
#5341 = DIRECTION('ref_axis',(1.,0.,3.49148133884313E-15)) ;
#5342 = DIRECTION('center_axis',(-3.49148133884313E-15,0.,1.)) ;
#5343 = DIRECTION('ref_axis',(1.,0.,3.49148133884313E-15)) ;
#5344 = DIRECTION('center_axis',(0.,-1.,0.)) ;
#5345 = DIRECTION('ref_axis',(-1.,0.,0.)) ;
#5346 = DIRECTION('',(0.,1.,0.)) ;
#5347 = DIRECTION('center_axis',(-3.38946600347724E-15,1.91189112624469E-17,
1.)) ;
#5348 = DIRECTION('ref_axis',(6.48028997475618E-32,1.,-1.91189112624469E-17)) ;
#5349 = DIRECTION('',(3.38946600347724E-15,-1.91189112624469E-17,-1.)) ;
#5350 = DIRECTION('center_axis',(-3.1843026467959E-15,0.342630345100702,0.93947030108257)) ;
#5351 = DIRECTION('ref_axis',(1.13665102922496E-30,0.93947030108257,-0.342630345100702)) ;
#5352 = DIRECTION('',(3.1843026467959E-15,-0.342630345100702,-0.93947030108257)) ;
#5353 = DIRECTION('center_axis',(-3.38946600347724E-15,0.,1.)) ;
#5354 = DIRECTION('ref_axis',(-1.,0.,-3.38946600347724E-15)) ;
#5355 = DIRECTION('',(3.38946600347724E-15,0.,-1.)) ;
#5356 = DIRECTION('center_axis',(0.,-1.,0.)) ;
#5357 = DIRECTION('ref_axis',(1.,0.,0.)) ;
#5358 = DIRECTION('',(0.,1.,0.)) ;
#5359 = DIRECTION('center_axis',(-3.49148133884313E-15,1.91189112624469E-17,
1.)) ;
#5360 = DIRECTION('ref_axis',(6.6753321891831E-32,1.,-1.91189112624469E-17)) ;
#5361 = DIRECTION('',(3.49148133884313E-15,-1.91189112624469E-17,-1.)) ;
#5362 = DIRECTION('center_axis',(-3.28014302462713E-15,0.342630345100702,
0.93947030108257)) ;
#5363 = DIRECTION('ref_axis',(1.24553608015764E-30,0.93947030108257,-0.342630345100702)) ;
#5364 = DIRECTION('',(3.28014302462713E-15,-0.342630345100702,-0.93947030108257)) ;
#5365 = DIRECTION('center_axis',(-3.49148133884313E-15,0.,1.)) ;
#5366 = DIRECTION('ref_axis',(1.,0.,3.49148133884313E-15)) ;
#5367 = DIRECTION('',(3.49148133884313E-15,0.,-1.)) ;
#5368 = DIRECTION('axis',(0.,0.,1.)) ;
#5369 = DIRECTION('refdir',(1.,0.,0.)) ;
#5370 = DIRECTION('center_axis',(6.88094734232038E-15,0.,-1.)) ;
#5371 = DIRECTION('ref_axis',(1.,0.,6.76707367390572E-15)) ;
#5372 = DIRECTION('center_axis',(1.,0.,6.88094734232038E-15)) ;
#5373 = DIRECTION('ref_axis',(6.88094734232038E-15,0.,-1.)) ;
#5374 = DIRECTION('center_axis',(-6.88094734232038E-15,0.,1.)) ;
#5375 = DIRECTION('ref_axis',(1.,0.,6.88094734232038E-15)) ;
#5376 = DIRECTION('center_axis',(0.,1.,0.)) ;
#5377 = DIRECTION('ref_axis',(4.62592926927148E-15,0.,-1.)) ;
#5378 = DIRECTION('center_axis',(0.,1.,0.)) ;
#5379 = DIRECTION('ref_axis',(4.62592926927148E-15,0.,-1.)) ;
#5380 = DIRECTION('center_axis',(6.88094734232038E-15,0.,-1.)) ;
#5381 = DIRECTION('ref_axis',(1.,0.,5.46571335200077E-15)) ;
#5382 = DIRECTION('center_axis',(0.93947030108257,-0.342630345100702,6.46444567142303E-15)) ;
#5383 = DIRECTION('ref_axis',(6.88775001098455E-15,1.86524785953259E-17,-1.)) ;
#5384 = DIRECTION('center_axis',(-6.88094734232038E-15,0.,1.)) ;
#5385 = DIRECTION('ref_axis',(1.,0.,6.88094734232038E-15)) ;
#5386 = DIRECTION('center_axis',(1.,0.,6.88094734232038E-15)) ;
#5387 = DIRECTION('ref_axis',(6.88094734232038E-15,0.,-1.)) ;
#5388 = DIRECTION('center_axis',(-6.88094734232038E-15,0.,1.)) ;
#5389 = DIRECTION('ref_axis',(-1.,0.,-5.46571335200077E-15)) ;
#5390 = DIRECTION('center_axis',(1.,0.,6.88094734232038E-15)) ;
#5391 = DIRECTION('ref_axis',(6.88094734232038E-15,0.,-1.)) ;
#5392 = DIRECTION('center_axis',(1.,0.,6.88094734232038E-15)) ;
#5393 = DIRECTION('ref_axis',(6.88094734232038E-15,0.,-1.)) ;
#5394 = DIRECTION('center_axis',(6.88094734232038E-15,0.,-1.)) ;
#5395 = DIRECTION('ref_axis',(-1.,0.,-6.88094734232038E-15)) ;
#5396 = DIRECTION('center_axis',(0.93947030108257,-0.342630345100702,6.46444567142303E-15)) ;
#5397 = DIRECTION('ref_axis',(6.61621824774427E-15,-7.25870098031252E-16,
-1.)) ;
#5398 = DIRECTION('center_axis',(0.93947030108257,-0.342630345100702,6.46444567142303E-15)) ;
#5399 = DIRECTION('ref_axis',(6.61621824774427E-15,-7.25870098031252E-16,
-1.)) ;
#5400 = DIRECTION('center_axis',(0.,-1.,0.)) ;
#5401 = DIRECTION('ref_axis',(-6.66133814775096E-15,0.,1.)) ;
#5402 = DIRECTION('center_axis',(1.,0.,6.88094734232038E-15)) ;
#5403 = DIRECTION('ref_axis',(6.88094734232038E-15,0.,-1.)) ;
#5404 = DIRECTION('center_axis',(0.,1.,0.)) ;
#5405 = DIRECTION('ref_axis',(-8.88178419700113E-15,0.,1.)) ;
#5406 = DIRECTION('center_axis',(-1.,0.,-6.98296267768627E-15)) ;
#5407 = DIRECTION('ref_axis',(-6.98296267768627E-15,0.,1.)) ;
#5408 = DIRECTION('center_axis',(-1.,0.,-6.98296267768627E-15)) ;
#5409 = DIRECTION('ref_axis',(-6.98296267768627E-15,0.,1.)) ;
#5410 = DIRECTION('center_axis',(1.,0.,6.88094734232038E-15)) ;
#5411 = DIRECTION('ref_axis',(6.88094734232038E-15,0.,-1.)) ;
#5412 = DIRECTION('center_axis',(-1.,0.,-6.98296267768627E-15)) ;
#5413 = DIRECTION('ref_axis',(-6.66133814775096E-15,0.,1.)) ;
#5414 = DIRECTION('center_axis',(0.,1.,0.)) ;
#5415 = DIRECTION('ref_axis',(4.62592926927148E-15,0.,-1.)) ;
#5416 = DIRECTION('center_axis',(0.,1.,0.)) ;
#5417 = DIRECTION('ref_axis',(4.62592926927148E-15,0.,-1.)) ;
#5418 = DIRECTION('center_axis',(1.,0.,6.98296267768627E-15)) ;
#5419 = DIRECTION('ref_axis',(-6.98296267768627E-15,0.,1.)) ;
#5420 = DIRECTION('center_axis',(0.,-1.,0.)) ;
#5421 = DIRECTION('ref_axis',(-9.25185853854296E-15,0.,1.)) ;
#5422 = DIRECTION('center_axis',(0.,-1.,0.)) ;
#5423 = DIRECTION('ref_axis',(-9.25185853854296E-15,0.,1.)) ;
#5424 = DIRECTION('center_axis',(-6.98296267768627E-15,0.,1.)) ;
#5425 = DIRECTION('ref_axis',(1.,0.,6.76707367390572E-15)) ;
#5426 = DIRECTION('center_axis',(0.,-1.,0.)) ;
#5427 = DIRECTION('ref_axis',(-9.25185853854296E-15,0.,1.)) ;
#5428 = DIRECTION('center_axis',(0.,-1.,0.)) ;
#5429 = DIRECTION('ref_axis',(-9.25185853854296E-15,0.,1.)) ;
#5430 = DIRECTION('center_axis',(6.98296267768627E-15,0.,-1.)) ;
#5431 = DIRECTION('ref_axis',(1.,0.,6.98296267768627E-15)) ;
#5432 = DIRECTION('center_axis',(-1.,0.,-6.98296267768627E-15)) ;
#5433 = DIRECTION('ref_axis',(-6.98296267768627E-15,0.,1.)) ;
#5434 = DIRECTION('center_axis',(-6.98296267768627E-15,0.,1.)) ;
#5435 = DIRECTION('ref_axis',(1.,0.,5.46571335200077E-15)) ;
#5436 = DIRECTION('center_axis',(-1.,0.,-6.98296267768627E-15)) ;
#5437 = DIRECTION('ref_axis',(-6.98296267768627E-15,0.,1.)) ;
#5438 = DIRECTION('center_axis',(6.98296267768627E-15,0.,-1.)) ;
#5439 = DIRECTION('ref_axis',(1.,0.,6.98296267768627E-15)) ;
#5440 = DIRECTION('center_axis',(-0.93947030108257,0.342630345100702,-6.56028604925426E-15)) ;
#5441 = DIRECTION('ref_axis',(-6.97778919960152E-15,1.41853431355683E-17,
1.)) ;
#5442 = DIRECTION('center_axis',(6.98296267768627E-15,0.,-1.)) ;
#5443 = DIRECTION('ref_axis',(-1.,0.,-5.46571335200077E-15)) ;
#5444 = DIRECTION('center_axis',(-0.93947030108257,0.342630345100702,-6.56028604925426E-15)) ;
#5445 = DIRECTION('ref_axis',(-7.24932096284181E-15,-7.30337233491011E-16,
1.)) ;
#5446 = DIRECTION('center_axis',(-0.93947030108257,0.342630345100702,-6.56028604925426E-15)) ;
#5447 = DIRECTION('ref_axis',(-7.24932096284181E-15,-7.30337233491011E-16,
1.)) ;
#5448 = DIRECTION('center_axis',(-6.98296267768627E-15,0.,1.)) ;
#5449 = DIRECTION('ref_axis',(-1.,0.,-6.98296267768627E-15)) ;
#5450 = DIRECTION('center_axis',(-1.,0.,-6.98296267768627E-15)) ;
#5451 = DIRECTION('ref_axis',(-6.98296267768627E-15,0.,1.)) ;
#5452 = DIRECTION('center_axis',(-1.,0.,-6.98296267768627E-15)) ;
#5453 = DIRECTION('ref_axis',(-6.98296267768627E-15,0.,1.)) ;
#5454 = DIRECTION('center_axis',(0.,-1.,0.)) ;
#5455 = DIRECTION('ref_axis',(4.62592926927148E-15,0.,-1.)) ;
#5456 = DIRECTION('',(0.,1.,0.)) ;
#5457 = DIRECTION('center_axis',(-1.,1.91189112624469E-17,-6.88094734232038E-15)) ;
#5458 = DIRECTION('ref_axis',(1.91189112624469E-17,1.,1.31556221639393E-31)) ;
#5459 = DIRECTION('',(1.,-1.91189112624469E-17,6.88094734232038E-15)) ;
#5460 = DIRECTION('center_axis',(-0.93947030108257,0.342630345100702,-6.46444567142303E-15)) ;
#5461 = DIRECTION('ref_axis',(0.342630345100702,0.93947030108257,-2.26638564151121E-29)) ;
#5462 = DIRECTION('',(0.93947030108257,-0.342630345100702,6.46444567142303E-15)) ;
#5463 = DIRECTION('center_axis',(-1.,0.,-6.88094734232038E-15)) ;
#5464 = DIRECTION('ref_axis',(6.88094734232038E-15,0.,-1.)) ;
#5465 = DIRECTION('',(1.,0.,6.88094734232038E-15)) ;
#5466 = DIRECTION('center_axis',(0.,-1.,0.)) ;
#5467 = DIRECTION('ref_axis',(-9.25185853854296E-15,0.,1.)) ;
#5468 = DIRECTION('',(0.,1.,0.)) ;
#5469 = DIRECTION('center_axis',(-1.,1.91189112624469E-17,-6.98296267768627E-15)) ;
#5470 = DIRECTION('ref_axis',(1.91189112624469E-17,1.,1.33506643783662E-31)) ;
#5471 = DIRECTION('',(1.,-1.91189112624469E-17,6.98296267768627E-15)) ;
#5472 = DIRECTION('center_axis',(-0.93947030108257,0.342630345100702,-6.56028604925426E-15)) ;
#5473 = DIRECTION('ref_axis',(0.342630345100702,0.93947030108257,-2.29769075252585E-29)) ;
#5474 = DIRECTION('',(0.93947030108257,-0.342630345100702,6.56028604925426E-15)) ;
#5475 = DIRECTION('center_axis',(-1.,0.,-6.98296267768627E-15)) ;
#5476 = DIRECTION('ref_axis',(-6.98296267768627E-15,0.,1.)) ;
#5477 = DIRECTION('',(1.,0.,6.98296267768627E-15)) ;
#5478 = DIRECTION('axis',(0.,0.,1.)) ;
#5479 = DIRECTION('refdir',(1.,0.,0.)) ;
#5480 = DIRECTION('center_axis',(1.,0.,1.03724286811635E-14)) ;
#5481 = DIRECTION('ref_axis',(-1.01506105108586E-14,0.,1.)) ;
#5482 = DIRECTION('center_axis',(-1.03724286811635E-14,0.,1.)) ;
#5483 = DIRECTION('ref_axis',(1.,0.,1.03724286811635E-14)) ;
#5484 = DIRECTION('center_axis',(-1.,0.,-1.03724286811635E-14)) ;
#5485 = DIRECTION('ref_axis',(-1.03724286811635E-14,0.,1.)) ;
#5486 = DIRECTION('center_axis',(0.,1.,0.)) ;
#5487 = DIRECTION('ref_axis',(1.,0.,9.25185853854296E-15)) ;
#5488 = DIRECTION('center_axis',(0.,1.,0.)) ;
#5489 = DIRECTION('ref_axis',(1.,0.,9.25185853854296E-15)) ;
#5490 = DIRECTION('center_axis',(1.,0.,1.03724286811635E-14)) ;
#5491 = DIRECTION('ref_axis',(-1.09314267040015E-14,0.,1.)) ;
#5492 = DIRECTION('center_axis',(-9.74458869605016E-15,-0.342630345100702,
0.93947030108257)) ;
#5493 = DIRECTION('ref_axis',(1.,2.61738882522057E-15,1.13270057821263E-14)) ;
#5494 = DIRECTION('center_axis',(-1.,0.,-1.03724286811635E-14)) ;
#5495 = DIRECTION('ref_axis',(-1.03724286811635E-14,0.,1.)) ;
#5496 = DIRECTION('center_axis',(-1.03724286811635E-14,0.,1.)) ;
#5497 = DIRECTION('ref_axis',(1.,0.,1.03724286811635E-14)) ;
#5498 = DIRECTION('center_axis',(-1.,0.,-1.03724286811635E-14)) ;
#5499 = DIRECTION('ref_axis',(1.09314267040015E-14,0.,-1.)) ;
#5500 = DIRECTION('center_axis',(-1.03724286811635E-14,0.,1.)) ;
#5501 = DIRECTION('ref_axis',(1.,0.,1.03724286811635E-14)) ;
#5502 = DIRECTION('center_axis',(-1.03724286811635E-14,0.,1.)) ;
#5503 = DIRECTION('ref_axis',(1.,0.,1.03724286811635E-14)) ;
#5504 = DIRECTION('center_axis',(1.,0.,1.03724286811635E-14)) ;
#5505 = DIRECTION('ref_axis',(1.03724286811635E-14,0.,-1.)) ;
#5506 = DIRECTION('center_axis',(-9.74458869605016E-15,-0.342630345100702,
0.93947030108257)) ;
#5507 = DIRECTION('ref_axis',(1.,2.61738882522057E-15,1.13270057821263E-14)) ;
#5508 = DIRECTION('center_axis',(-9.74458869605016E-15,-0.342630345100702,
0.93947030108257)) ;
#5509 = DIRECTION('ref_axis',(1.,2.61738882522057E-15,1.13270057821263E-14)) ;
#5510 = DIRECTION('center_axis',(0.,-1.,0.)) ;
#5511 = DIRECTION('ref_axis',(-1.,0.,-1.33226762955019E-14)) ;
#5512 = DIRECTION('center_axis',(-1.03724286811635E-14,0.,1.)) ;
#5513 = DIRECTION('ref_axis',(1.,0.,1.03724286811635E-14)) ;
#5514 = DIRECTION('center_axis',(0.,1.,0.)) ;
#5515 = DIRECTION('ref_axis',(-1.,0.,-1.77635683940026E-14)) ;
#5516 = DIRECTION('center_axis',(1.04744440165294E-14,0.,-1.)) ;
#5517 = DIRECTION('ref_axis',(-1.,0.,-1.04744440165294E-14)) ;
#5518 = DIRECTION('center_axis',(1.04744440165294E-14,0.,-1.)) ;
#5519 = DIRECTION('ref_axis',(-1.,0.,-1.04744440165294E-14)) ;
#5520 = DIRECTION('center_axis',(-1.03724286811635E-14,0.,1.)) ;
#5521 = DIRECTION('ref_axis',(1.,0.,1.03724286811635E-14)) ;
#5522 = DIRECTION('center_axis',(1.04744440165294E-14,0.,-1.)) ;
#5523 = DIRECTION('ref_axis',(-1.,0.,-1.11022302462516E-14)) ;
#5524 = DIRECTION('center_axis',(0.,1.,0.)) ;
#5525 = DIRECTION('ref_axis',(1.,0.,9.25185853854296E-15)) ;
#5526 = DIRECTION('center_axis',(0.,1.,0.)) ;
#5527 = DIRECTION('ref_axis',(1.,0.,9.25185853854296E-15)) ;
#5528 = DIRECTION('center_axis',(-1.04744440165294E-14,0.,1.)) ;
#5529 = DIRECTION('ref_axis',(-1.,0.,-1.04744440165294E-14)) ;
#5530 = DIRECTION('center_axis',(0.,-1.,0.)) ;
#5531 = DIRECTION('ref_axis',(-1.,0.,-9.25185853854296E-15)) ;
#5532 = DIRECTION('center_axis',(0.,-1.,0.)) ;
#5533 = DIRECTION('ref_axis',(-1.,0.,-9.25185853854296E-15)) ;
#5534 = DIRECTION('center_axis',(-1.,0.,-1.04744440165294E-14)) ;
#5535 = DIRECTION('ref_axis',(-1.01506105108586E-14,0.,1.)) ;
#5536 = DIRECTION('center_axis',(0.,-1.,0.)) ;
#5537 = DIRECTION('ref_axis',(-1.,0.,-9.25185853854296E-15)) ;
#5538 = DIRECTION('center_axis',(0.,-1.,0.)) ;
#5539 = DIRECTION('ref_axis',(-1.,0.,-9.25185853854296E-15)) ;
#5540 = DIRECTION('center_axis',(1.,0.,1.04744440165294E-14)) ;
#5541 = DIRECTION('ref_axis',(-1.04744440165294E-14,0.,1.)) ;
#5542 = DIRECTION('center_axis',(1.04744440165294E-14,0.,-1.)) ;
#5543 = DIRECTION('ref_axis',(-1.,0.,-1.04744440165294E-14)) ;
#5544 = DIRECTION('center_axis',(-1.,0.,-1.04744440165294E-14)) ;
#5545 = DIRECTION('ref_axis',(-1.09314267040015E-14,0.,1.)) ;
#5546 = DIRECTION('center_axis',(1.04744440165294E-14,0.,-1.)) ;
#5547 = DIRECTION('ref_axis',(-1.,0.,-1.04744440165294E-14)) ;
#5548 = DIRECTION('center_axis',(1.,0.,1.04744440165294E-14)) ;
#5549 = DIRECTION('ref_axis',(-1.04744440165294E-14,0.,1.)) ;
#5550 = DIRECTION('center_axis',(9.8404290738814E-15,0.342630345100702,-0.93947030108257)) ;
#5551 = DIRECTION('ref_axis',(-1.,-2.58455100348968E-15,-1.14170449707433E-14)) ;
#5552 = DIRECTION('center_axis',(1.,0.,1.04744440165294E-14)) ;
#5553 = DIRECTION('ref_axis',(1.09314267040015E-14,0.,-1.)) ;
#5554 = DIRECTION('center_axis',(9.8404290738814E-15,0.342630345100702,-0.93947030108257)) ;
#5555 = DIRECTION('ref_axis',(-1.,-2.58455100348968E-15,-1.14170449707433E-14)) ;
#5556 = DIRECTION('center_axis',(9.8404290738814E-15,0.342630345100702,-0.93947030108257)) ;
#5557 = DIRECTION('ref_axis',(-1.,-2.58455100348968E-15,-1.14170449707433E-14)) ;
#5558 = DIRECTION('center_axis',(-1.,0.,-1.04744440165294E-14)) ;
#5559 = DIRECTION('ref_axis',(1.04744440165294E-14,0.,-1.)) ;
#5560 = DIRECTION('center_axis',(1.04744440165294E-14,0.,-1.)) ;
#5561 = DIRECTION('ref_axis',(-1.,0.,-1.04744440165294E-14)) ;
#5562 = DIRECTION('center_axis',(1.04744440165294E-14,0.,-1.)) ;
#5563 = DIRECTION('ref_axis',(-1.,0.,-1.04744440165294E-14)) ;
#5564 = DIRECTION('center_axis',(0.,-1.,0.)) ;
#5565 = DIRECTION('ref_axis',(1.,0.,9.25185853854296E-15)) ;
#5566 = DIRECTION('',(0.,1.,0.)) ;
#5567 = DIRECTION('center_axis',(1.03724286811635E-14,1.91189112624469E-17,
-1.)) ;
#5568 = DIRECTION('ref_axis',(-1.98309543531224E-31,1.,1.91189112624469E-17)) ;
#5569 = DIRECTION('',(-1.03724286811635E-14,-1.91189112624469E-17,1.)) ;
#5570 = DIRECTION('center_axis',(9.74458869605016E-15,0.342630345100702,-0.93947030108257)) ;
#5571 = DIRECTION('ref_axis',(-4.62592926927152E-15,0.93947030108257,0.342630345100702)) ;
#5572 = DIRECTION('',(-9.74458869605016E-15,-0.342630345100702,0.93947030108257)) ;
#5573 = DIRECTION('center_axis',(1.03724286811635E-14,0.,-1.)) ;
#5574 = DIRECTION('ref_axis',(1.,0.,1.03724286811635E-14)) ;
#5575 = DIRECTION('',(-1.03724286811635E-14,0.,1.)) ;
#5576 = DIRECTION('center_axis',(0.,-1.,0.)) ;
#5577 = DIRECTION('ref_axis',(-1.,0.,-9.25185853854296E-15)) ;
#5578 = DIRECTION('',(0.,1.,0.)) ;
#5579 = DIRECTION('center_axis',(1.04744440165294E-14,1.91189112624469E-17,
-1.)) ;
#5580 = DIRECTION('ref_axis',(-2.00259965675493E-31,1.,1.91189112624469E-17)) ;
#5581 = DIRECTION('',(-1.04744440165294E-14,-1.91189112624469E-17,1.)) ;
#5582 = DIRECTION('center_axis',(9.8404290738814E-15,0.342630345100702,-0.93947030108257)) ;
#5583 = DIRECTION('ref_axis',(-4.62592926927152E-15,0.93947030108257,0.342630345100702)) ;
#5584 = DIRECTION('',(-9.8404290738814E-15,-0.342630345100702,0.93947030108257)) ;
#5585 = DIRECTION('center_axis',(1.04744440165294E-14,0.,-1.)) ;
#5586 = DIRECTION('ref_axis',(-1.,0.,-1.04744440165294E-14)) ;
#5587 = DIRECTION('',(-1.04744440165294E-14,0.,1.)) ;
#5588 = DIRECTION('',(0.,0.,1.)) ;
#5589 = DIRECTION('',(1.,0.,0.)) ;
#5590 = DIRECTION('',(0.,0.,1.)) ;
#5591 = DIRECTION('',(1.,0.,0.)) ;
#5592 = DIRECTION('',(0.,0.,1.)) ;
#5593 = DIRECTION('',(1.,0.,0.)) ;
#5594 = DIRECTION('',(0.,0.,1.)) ;
#5595 = DIRECTION('',(1.,0.,0.)) ;
#5596 = DIRECTION('',(0.,0.,1.)) ;
#5597 = DIRECTION('',(1.,0.,0.)) ;
#5598 = DIRECTION('',(0.,0.,1.)) ;
#5599 = DIRECTION('',(1.,0.,0.)) ;
#5600 = DIRECTION('',(0.,0.,1.)) ;
#5601 = DIRECTION('',(1.,0.,0.)) ;
#5602 = DIRECTION('',(0.,0.,1.)) ;
#5603 = DIRECTION('',(1.,0.,0.)) ;
#5604 = CARTESIAN_POINT('',(0.,0.,0.)) ;
#5605 = CARTESIAN_POINT('',(0.,0.,0.)) ;
#5606 = CARTESIAN_POINT('',(0.,0.,0.)) ;
#5607 = CARTESIAN_POINT('Origin',(23.47768801576,48.8830586252741,68.2224337400009)) ;
#5608 = CARTESIAN_POINT('',(23.47768801576,43.9861713801022,31.272433740001)) ;
#5609 = CARTESIAN_POINT('',(23.47768801576,43.9861713801022,105.172433740001)) ;
#5610 = CARTESIAN_POINT('Origin',(23.47768801576,43.9861713801022,68.2224337400009)) ;
#5611 = CARTESIAN_POINT('Origin',(23.47768801576,43.9861713801022,68.2224337400009)) ;
#5612 = CARTESIAN_POINT('',(23.4776880157599,48.8830586252741,103.222433740001)) ;
#5613 = CARTESIAN_POINT('Origin',(23.47768801576,48.8830586252741,110.346024686649)) ;
#5614 = CARTESIAN_POINT('Origin',(23.47768801576,48.8830586252741,68.2224337400009)) ;
#5615 = CARTESIAN_POINT('Origin',(23.47768801576,48.8830586252741,68.2224337400009)) ;
#5616 = CARTESIAN_POINT('',(23.4776880157599,48.8830586252741,103.072433740001)) ;
#5617 = CARTESIAN_POINT('Origin',(23.47768801576,48.8830586252741,68.2224337400009)) ;
#5618 = CARTESIAN_POINT('',(23.47768801576,43.8830586252739,105.063494491831)) ;
#5619 = CARTESIAN_POINT('Origin',(23.47768801576,48.8830586252741,110.346024686649)) ;
#5620 = CARTESIAN_POINT('',(23.47768801576,43.8830586252739,31.3813729881705)) ;
#5621 = CARTESIAN_POINT('Origin',(23.47768801576,43.8830586252739,68.2224337400009)) ;
#5622 = CARTESIAN_POINT('Origin',(23.47768801576,43.8830586252739,68.2224337400009)) ;
#5623 = CARTESIAN_POINT('Origin',(23.47768801576,43.8830586252739,68.2224337400009)) ;
#5624 = CARTESIAN_POINT('',(23.47768801576,43.8830586252739,31.3813729881706)) ;
#5625 = CARTESIAN_POINT('Origin',(58.3276880157596,48.8830586252741,68.2224337400009)) ;
#5626 = CARTESIAN_POINT('',(0.,0.,0.)) ;
#5627 = CARTESIAN_POINT('Origin',(23.47768801576,52.6592998081416,68.2224337400009)) ;
#5628 = CARTESIAN_POINT('',(23.47768801576,41.1202437104732,27.21194648433)) ;
#5629 = CARTESIAN_POINT('',(23.47768801576,41.1202437104732,109.232920995672)) ;
#5630 = CARTESIAN_POINT('Origin',(23.47768801576,41.1202437104732,68.2224337400009)) ;
#5631 = CARTESIAN_POINT('Origin',(23.47768801576,41.1202437104732,68.2224337400009)) ;
#5632 = CARTESIAN_POINT('',(23.47768801576,43.9499264022543,105.206876611489)) ;
#5633 = CARTESIAN_POINT('Origin',(23.47768801576,52.6592998081416,114.335646300933)) ;
#5634 = CARTESIAN_POINT('',(23.47768801576,43.9499264022543,31.2379908685129)) ;
#5635 = CARTESIAN_POINT('Origin',(23.47768801576,43.9499264022543,68.2224337400009)) ;
#5636 = CARTESIAN_POINT('Origin',(23.47768801576,43.9499264022543,68.2224337400009)) ;
#5637 = CARTESIAN_POINT('Origin',(23.47768801576,41.1202437104732,68.2224337400009)) ;
#5638 = CARTESIAN_POINT('',(23.47768801576,40.9830586252741,27.272611568183)) ;
#5639 = CARTESIAN_POINT('',(23.47768801576,41.1202437104732,27.21194648433)) ;
#5640 = CARTESIAN_POINT('',(23.47768801576,40.9830586252741,109.172255911819)) ;
#5641 = CARTESIAN_POINT('Origin',(23.47768801576,40.9830586252741,68.2224337400009)) ;
#5642 = CARTESIAN_POINT('Origin',(23.47768801576,40.9830586252741,68.2224337400009)) ;
#5643 = CARTESIAN_POINT('Origin',(23.47768801576,52.6592998081416,68.2224337400009)) ;
#5644 = CARTESIAN_POINT('',(23.47768801576,43.8468128472507,31.3469309620732)) ;
#5645 = CARTESIAN_POINT('',(23.47768801576,43.8468128472507,105.097936517929)) ;
#5646 = CARTESIAN_POINT('Origin',(23.47768801576,43.8468128472507,68.2224337400009)) ;
#5647 = CARTESIAN_POINT('Origin',(23.47768801576,43.8468128472507,68.2224337400009)) ;
#5648 = CARTESIAN_POINT('Origin',(23.47768801576,52.6592998081416,114.335646300933)) ;
#5649 = CARTESIAN_POINT('Origin',(23.47768801576,43.9499264022543,68.2224337400009)) ;
#5650 = CARTESIAN_POINT('',(23.47768801576,43.9499264022543,31.2379908685129)) ;
#5651 = CARTESIAN_POINT('',(0.,0.,0.)) ;
#5652 = CARTESIAN_POINT('Origin',(23.47768801576,60.3830586252741,68.2224337400009)) ;
#5653 = CARTESIAN_POINT('',(58.87768801576,60.3830586252741,68.2224337400009)) ;
#5654 = CARTESIAN_POINT('Origin',(59.22768801576,60.3830586252741,68.2224337400009)) ;
#5655 = CARTESIAN_POINT('Origin',(23.47768801576,60.3830586252741,68.2224337400009)) ;
#5656 = CARTESIAN_POINT('',(0.,0.,0.)) ;
#5657 = CARTESIAN_POINT('Origin',(23.47768801576,61.7830586252741,68.2224337400009)) ;
#5658 = CARTESIAN_POINT('',(58.87768801576,61.7830586252741,68.2224337400009)) ;
#5659 = CARTESIAN_POINT('Origin',(59.22768801576,61.7830586252741,68.2224337400009)) ;
#5660 = CARTESIAN_POINT('Origin',(23.47768801576,61.7830586252741,68.2224337400009)) ;
#5661 = CARTESIAN_POINT('',(0.,0.,0.)) ;
#5662 = CARTESIAN_POINT('Origin',(23.47768801576,63.1830586252741,68.2224337400009)) ;
#5663 = CARTESIAN_POINT('',(58.87768801576,63.1830586252741,68.2224337400009)) ;
#5664 = CARTESIAN_POINT('Origin',(59.22768801576,63.1830586252741,68.2224337400009)) ;
#5665 = CARTESIAN_POINT('Origin',(23.47768801576,63.1830586252741,68.2224337400009)) ;
#5666 = CARTESIAN_POINT('',(0.,0.,0.)) ;
#5667 = CARTESIAN_POINT('Origin',(23.47768801576,64.5830586252741,68.2224337400009)) ;
#5668 = CARTESIAN_POINT('',(58.87768801576,64.5830586252741,68.2224337400009)) ;
#5669 = CARTESIAN_POINT('Origin',(59.22768801576,64.5830586252741,68.2224337400009)) ;
#5670 = CARTESIAN_POINT('Origin',(23.47768801576,64.5830586252741,68.2224337400009)) ;
#5671 = CARTESIAN_POINT('',(0.,0.,0.)) ;
#5672 = CARTESIAN_POINT('Origin',(23.47768801576,65.9830586252741,68.2224337400009)) ;
#5673 = CARTESIAN_POINT('',(58.87768801576,65.9830586252741,68.2224337400009)) ;
#5674 = CARTESIAN_POINT('Origin',(59.22768801576,65.9830586252741,68.2224337400009)) ;
#5675 = CARTESIAN_POINT('Origin',(23.47768801576,65.9830586252741,68.2224337400009)) ;
#5676 = CARTESIAN_POINT('',(0.,0.,0.)) ;
#5677 = CARTESIAN_POINT('Origin',(23.47768801576,67.3831179463143,68.2224337400009)) ;
#5678 = CARTESIAN_POINT('',(-11.5991264456068,67.3831179463143,68.2224337400009)) ;
#5679 = CARTESIAN_POINT('Origin',(-11.9491264456068,67.3831179463143,68.2224337400009)) ;
#5680 = CARTESIAN_POINT('Origin',(23.47768801576,67.3831179463143,68.2224337400009)) ;
#5681 = CARTESIAN_POINT('',(0.,0.,0.)) ;
#5682 = CARTESIAN_POINT('Origin',(23.47768801576,67.3831179463143,68.2224337400009)) ;
#5683 = CARTESIAN_POINT('',(-9.5991264456068,67.3831179463143,68.2224337400009)) ;
#5684 = CARTESIAN_POINT('Origin',(-9.9491264456068,67.3831179463143,68.2224337400009)) ;
#5685 = CARTESIAN_POINT('Origin',(23.47768801576,67.3831179463143,68.2224337400009)) ;
#5686 = CARTESIAN_POINT('',(0.,0.,0.)) ;
#5687 = CARTESIAN_POINT('Origin',(23.47768801576,67.3831179463143,68.2224337400009)) ;
#5688 = CARTESIAN_POINT('',(-7.5991264456068,67.3831179463143,68.2224337400009)) ;
#5689 = CARTESIAN_POINT('Origin',(-7.9491264456068,67.3831179463143,68.2224337400009)) ;
#5690 = CARTESIAN_POINT('Origin',(23.47768801576,67.3831179463143,68.2224337400009)) ;
#5691 = CARTESIAN_POINT('',(0.,0.,0.)) ;
#5692 = CARTESIAN_POINT('Origin',(23.47768801576,67.3831179463143,68.2224337400009)) ;
#5693 = CARTESIAN_POINT('',(-5.5991264456068,67.3831179463143,68.2224337400009)) ;
#5694 = CARTESIAN_POINT('Origin',(-5.9491264456068,67.3831179463143,68.2224337400009)) ;
#5695 = CARTESIAN_POINT('Origin',(23.47768801576,67.3831179463143,68.2224337400009)) ;
#5696 = CARTESIAN_POINT('',(0.,0.,0.)) ;
#5697 = CARTESIAN_POINT('Origin',(23.47768801576,67.3831179463143,68.2224337400009)) ;
#5698 = CARTESIAN_POINT('',(-3.5991264456068,67.3831179463143,68.2224337400009)) ;
#5699 = CARTESIAN_POINT('Origin',(-3.9491264456068,67.3831179463143,68.2224337400009)) ;
#5700 = CARTESIAN_POINT('Origin',(23.47768801576,67.3831179463143,68.2224337400009)) ;
#5701 = CARTESIAN_POINT('',(0.,0.,0.)) ;
#5702 = CARTESIAN_POINT('Origin',(23.47768801576,67.3831179463143,68.2224337400009)) ;
#5703 = CARTESIAN_POINT('',(-1.5991264456068,67.3831179463143,68.2224337400009)) ;
#5704 = CARTESIAN_POINT('Origin',(-1.9491264456068,67.3831179463143,68.2224337400009)) ;
#5705 = CARTESIAN_POINT('Origin',(23.47768801576,67.3831179463143,68.2224337400009)) ;
#5706 = CARTESIAN_POINT('',(0.,0.,0.)) ;
#5707 = CARTESIAN_POINT('Origin',(23.47768801576,67.3831179463143,68.2224337400009)) ;
#5708 = CARTESIAN_POINT('',(0.400873554393198,67.3831179463143,68.2224337400009)) ;
#5709 = CARTESIAN_POINT('Origin',(0.0508735543931991,67.3831179463143,68.2224337400009)) ;
#5710 = CARTESIAN_POINT('Origin',(23.47768801576,67.3831179463143,68.2224337400009)) ;
#5711 = CARTESIAN_POINT('',(0.,0.,0.)) ;
#5712 = CARTESIAN_POINT('Origin',(23.47768801576,67.3831179463143,68.2224337400009)) ;
#5713 = CARTESIAN_POINT('',(2.4008735543932,67.3831179463143,68.2224337400009)) ;
#5714 = CARTESIAN_POINT('Origin',(2.0508735543932,67.3831179463143,68.2224337400009)) ;
#5715 = CARTESIAN_POINT('Origin',(23.47768801576,67.3831179463143,68.2224337400009)) ;
#5716 = CARTESIAN_POINT('',(0.,0.,0.)) ;
#5717 = CARTESIAN_POINT('Origin',(23.47768801576,67.3831179463143,68.2224337400009)) ;
#5718 = CARTESIAN_POINT('',(4.4008735543932,67.3831179463143,68.2224337400009)) ;
#5719 = CARTESIAN_POINT('Origin',(4.0508735543932,67.3831179463143,68.2224337400009)) ;
#5720 = CARTESIAN_POINT('Origin',(23.47768801576,67.3831179463143,68.2224337400009)) ;
#5721 = CARTESIAN_POINT('',(0.,0.,0.)) ;
#5722 = CARTESIAN_POINT('Origin',(23.47768801576,67.3831179463143,68.2224337400009)) ;
#5723 = CARTESIAN_POINT('',(6.4008735543932,67.3831179463143,68.2224337400009)) ;
#5724 = CARTESIAN_POINT('Origin',(6.0508735543932,67.3831179463143,68.2224337400009)) ;
#5725 = CARTESIAN_POINT('Origin',(23.47768801576,67.3831179463143,68.2224337400009)) ;
#5726 = CARTESIAN_POINT('',(0.,0.,0.)) ;
#5727 = CARTESIAN_POINT('Origin',(23.47768801576,66.6831179463143,68.2224337400009)) ;
#5728 = CARTESIAN_POINT('',(8.4008735543932,66.6831179463143,68.2224337400009)) ;
#5729 = CARTESIAN_POINT('Origin',(8.0508735543932,66.6831179463143,68.2224337400009)) ;
#5730 = CARTESIAN_POINT('Origin',(23.47768801576,66.6831179463143,68.2224337400009)) ;
#5731 = CARTESIAN_POINT('',(0.,0.,0.)) ;
#5732 = CARTESIAN_POINT('Origin',(23.47768801576,65.9831179463143,68.2224337400009)) ;
#5733 = CARTESIAN_POINT('',(10.4008735543932,65.9831179463143,68.2224337400009)) ;
#5734 = CARTESIAN_POINT('Origin',(10.0508735543932,65.9831179463143,68.2224337400009)) ;
#5735 = CARTESIAN_POINT('Origin',(23.47768801576,65.9831179463143,68.2224337400009)) ;
#5736 = CARTESIAN_POINT('',(0.,0.,0.)) ;
#5737 = CARTESIAN_POINT('Origin',(23.47768801576,65.2831179463143,68.2224337400009)) ;
#5738 = CARTESIAN_POINT('',(12.4008735543932,65.2831179463143,68.2224337400009)) ;
#5739 = CARTESIAN_POINT('Origin',(12.0508735543932,65.2831179463143,68.2224337400009)) ;
#5740 = CARTESIAN_POINT('Origin',(23.47768801576,65.2831179463143,68.2224337400009)) ;
#5741 = CARTESIAN_POINT('',(0.,0.,0.)) ;
#5742 = CARTESIAN_POINT('Origin',(23.47768801576,64.5831179463143,68.2224337400009)) ;
#5743 = CARTESIAN_POINT('',(14.4008735543932,64.5831179463143,68.2224337400009)) ;
#5744 = CARTESIAN_POINT('Origin',(14.0508735543932,64.5831179463143,68.2224337400009)) ;
#5745 = CARTESIAN_POINT('Origin',(23.47768801576,64.5831179463143,68.2224337400009)) ;
#5746 = CARTESIAN_POINT('',(0.,0.,0.)) ;
#5747 = CARTESIAN_POINT('Origin',(23.47768801576,63.8831179463143,68.2224337400009)) ;
#5748 = CARTESIAN_POINT('',(16.4008735543932,63.8831179463143,68.2224337400009)) ;
#5749 = CARTESIAN_POINT('Origin',(16.0508735543932,63.8831179463143,68.2224337400009)) ;
#5750 = CARTESIAN_POINT('Origin',(23.47768801576,63.8831179463143,68.2224337400009)) ;
#5751 = CARTESIAN_POINT('',(0.,0.,0.)) ;
#5752 = CARTESIAN_POINT('Origin',(23.47768801576,63.1831179463143,68.2224337400009)) ;
#5753 = CARTESIAN_POINT('',(18.4008735543932,63.1831179463143,68.2224337400009)) ;
#5754 = CARTESIAN_POINT('Origin',(18.0508735543932,63.1831179463143,68.2224337400009)) ;
#5755 = CARTESIAN_POINT('Origin',(23.47768801576,63.1831179463143,68.2224337400009)) ;
#5756 = CARTESIAN_POINT('',(0.,0.,0.)) ;
#5757 = CARTESIAN_POINT('Origin',(23.47768801576,62.6831179463143,68.2224337400009)) ;
#5758 = CARTESIAN_POINT('',(20.4008735543932,62.6831179463143,68.2224337400009)) ;
#5759 = CARTESIAN_POINT('Origin',(20.0508735543932,62.6831179463143,68.2224337400009)) ;
#5760 = CARTESIAN_POINT('Origin',(23.47768801576,62.6831179463143,68.2224337400009)) ;
#5761 = CARTESIAN_POINT('',(0.,0.,0.)) ;
#5762 = CARTESIAN_POINT('',(0.,0.,0.)) ;
#5763 = CARTESIAN_POINT('',(0.,0.,0.)) ;
#5764 = CARTESIAN_POINT('',(0.,0.,0.)) ;
#5765 = CARTESIAN_POINT('',(0.,0.,0.)) ;
#5766 = CARTESIAN_POINT('',(0.,0.,0.)) ;
#5767 = CARTESIAN_POINT('',(0.,0.,0.)) ;
#5768 = CARTESIAN_POINT('',(0.,0.,0.)) ;
#5769 = CARTESIAN_POINT('',(0.,0.,0.)) ;
#5770 = CARTESIAN_POINT('',(0.,0.,0.)) ;
#5771 = CARTESIAN_POINT('',(0.,0.,0.)) ;
#5772 = CARTESIAN_POINT('',(0.,0.,0.)) ;
#5773 = CARTESIAN_POINT('',(0.,0.,0.)) ;
#5774 = CARTESIAN_POINT('',(0.,0.,0.)) ;
#5775 = CARTESIAN_POINT('',(0.,0.,0.)) ;
#5776 = CARTESIAN_POINT('',(0.,0.,0.)) ;
#5777 = CARTESIAN_POINT('',(0.,0.,0.)) ;
#5778 = CARTESIAN_POINT('',(0.,0.,0.)) ;
#5779 = CARTESIAN_POINT('',(0.,0.,0.)) ;
#5780 = CARTESIAN_POINT('',(0.,0.,0.)) ;
#5781 = CARTESIAN_POINT('',(0.,0.,0.)) ;
#5782 = CARTESIAN_POINT('',(0.,0.,0.)) ;
#5783 = CARTESIAN_POINT('',(0.,0.,0.)) ;
#5784 = CARTESIAN_POINT('',(0.,0.,0.)) ;
#5785 = CARTESIAN_POINT('',(0.,0.,0.)) ;
#5786 = CARTESIAN_POINT('',(0.,0.,0.)) ;
#5787 = CARTESIAN_POINT('Origin',(23.47768801576,43.8830586252741,68.2224337400009)) ;
#5788 = CARTESIAN_POINT('',(31.07768801576,59.8830586252741,68.2224337400009)) ;
#5789 = CARTESIAN_POINT('Origin',(23.47768801576,59.8830586252741,68.2224337400009)) ;
#5790 = CARTESIAN_POINT('',(31.0776880612976,45.9361079682058,68.2224337399987)) ;
#5791 = CARTESIAN_POINT('',(31.07768801576,43.8830586252741,68.2224337400009)) ;
#5792 = CARTESIAN_POINT('',(31.0707352866625,45.3830586252742,67.8974209876918)) ;
#5793 = CARTESIAN_POINT('Ctrl Pts',(31.07768801576,45.9361079682046,68.2224337400009)) ;
#5794 = CARTESIAN_POINT('Ctrl Pts',(31.07768801576,45.7519411862255,68.1142267889447)) ;
#5795 = CARTESIAN_POINT('Ctrl Pts',(31.0753771201502,45.5676059004178,68.0058651472121)) ;
#5796 = CARTESIAN_POINT('Ctrl Pts',(31.070735276979,45.3830586252741,67.8974209881066)) ;
#5797 = CARTESIAN_POINT('',(31.07768801576,45.3830586252741,68.2224337400009)) ;
#5798 = CARTESIAN_POINT('Origin',(23.47768801576,45.3830586252741,68.2224337400009)) ;
#5799 = CARTESIAN_POINT('',(31.07768801576,43.8830586252741,68.2224337400009)) ;
#5800 = CARTESIAN_POINT('',(31.07768801576,43.8830586252741,68.2224337400009)) ;
#5801 = CARTESIAN_POINT('Origin',(23.47768801576,43.8830586252741,68.2224337400009)) ;
#5802 = CARTESIAN_POINT('',(31.0742800734864,45.3830634900505,68.4500118893126)) ;
#5803 = CARTESIAN_POINT('Origin',(23.47768801576,45.3830586252741,68.2224337400009)) ;
#5804 = CARTESIAN_POINT('',(27.6340951062153,57.8256696109516,74.5851579545834)) ;
#5805 = CARTESIAN_POINT('Ctrl Pts',(31.0742801230022,45.3830652731003,68.4500124151661)) ;
#5806 = CARTESIAN_POINT('Ctrl Pts',(31.0705756008784,45.5935267840764,68.5736831572555)) ;
#5807 = CARTESIAN_POINT('Ctrl Pts',(31.0638548672636,45.8038922449875,68.6971313448079)) ;
#5808 = CARTESIAN_POINT('Ctrl Pts',(31.0518691119314,46.0632318317031,68.8490202361335)) ;
#5809 = CARTESIAN_POINT('Ctrl Pts',(31.0494392191971,46.1122612415161,68.8777284508602)) ;
#5810 = CARTESIAN_POINT('Ctrl Pts',(31.0351342059633,46.3827042839367,69.0360189559014)) ;
#5811 = CARTESIAN_POINT('Ctrl Pts',(31.020087358527,46.6040125923428,69.1653747748633)) ;
#5812 = CARTESIAN_POINT('Ctrl Pts',(30.9986034331019,46.8632622432151,69.3162007814499)) ;
#5813 = CARTESIAN_POINT('Ctrl Pts',(30.9953693582315,46.9011261856475,69.3382131230647)) ;
#5814 = CARTESIAN_POINT('Ctrl Pts',(30.9715704181779,47.1717033808735,69.495396997657)) ;
#5815 = CARTESIAN_POINT('Ctrl Pts',(30.9474582703363,47.4044689603727,69.6300128694532)) ;
#5816 = CARTESIAN_POINT('Ctrl Pts',(30.9165145207437,47.663862891896,69.7793873192818)) ;
#5817 = CARTESIAN_POINT('Ctrl Pts',(30.9132972664022,47.6904386808295,69.7946800230084)) ;
#5818 = CARTESIAN_POINT('Ctrl Pts',(30.8800288137658,47.9612998636033,69.9504289150583)) ;
#5819 = CARTESIAN_POINT('Ctrl Pts',(30.8460515474602,48.2057236046572,70.0899969837708)) ;
#5820 = CARTESIAN_POINT('Ctrl Pts',(30.8058460215849,48.4649882125099,70.2369260769358)) ;
#5821 = CARTESIAN_POINT('Ctrl Pts',(30.8034830172247,48.4801277704431,70.2455023164062)) ;
#5822 = CARTESIAN_POINT('Ctrl Pts',(30.7609672635063,48.7507815722807,70.3987560508298)) ;
#5823 = CARTESIAN_POINT('Ctrl Pts',(30.7165304066699,49.0060603871242,70.5422753814737)) ;
#5824 = CARTESIAN_POINT('Ctrl Pts',(30.6672297149442,49.2650911286699,70.6862711816059)) ;
#5825 = CARTESIAN_POINT('Ctrl Pts',(30.666520422233,49.268813158774,70.6883399479886)) ;
#5826 = CARTESIAN_POINT('Ctrl Pts',(30.6163861031706,49.5315653220715,70.8343594519423)) ;
#5827 = CARTESIAN_POINT('Ctrl Pts',(30.5626668547145,49.7905771610405,70.9767535845282)) ;
#5828 = CARTESIAN_POINT('Ctrl Pts',(30.5029239276412,50.0572510953406,71.121757941137)) ;
#5829 = CARTESIAN_POINT('Ctrl Pts',(30.5012000878133,50.0649289262866,71.1259313834614)) ;
#5830 = CARTESIAN_POINT('Ctrl Pts',(30.4429225840978,50.3239244418443,71.2666667874793)) ;
#5831 = CARTESIAN_POINT('Ctrl Pts',(30.3824337723248,50.57540159488,71.4014830392169)) ;
#5832 = CARTESIAN_POINT('Ctrl Pts',(30.3131067557725,50.8461423400815,71.5446584556825)) ;
#5833 = CARTESIAN_POINT('Ctrl Pts',(30.3081912119758,50.8652509230901,71.5547530784007)) ;
#5834 = CARTESIAN_POINT('Ctrl Pts',(30.2411699989914,51.1245997230081,71.6916179346065)) ;
#5835 = CARTESIAN_POINT('Ctrl Pts',(30.1754230730788,51.3650618940604,71.8169064463964)) ;
#5836 = CARTESIAN_POINT('Ctrl Pts',(30.0975881230115,51.635843742555,71.9556952593753)) ;
#5837 = CARTESIAN_POINT('Ctrl Pts',(30.088754982762,51.6663832990536,71.9713156300781)) ;
#5838 = CARTESIAN_POINT('Ctrl Pts',(30.0010861726626,51.9676379850986,72.1250705521229)) ;
#5839 = CARTESIAN_POINT('Ctrl Pts',(29.9180156669,52.238164456489,72.2606837295049)) ;
#5840 = CARTESIAN_POINT('Ctrl Pts',(29.7606847862324,52.7256472364709,72.5003125758719)) ;
#5841 = CARTESIAN_POINT('Ctrl Pts',(29.6880049010229,52.9427458528976,72.6051556822608)) ;
#5842 = CARTESIAN_POINT('Ctrl Pts',(29.5942325442125,53.2131562545788,72.7334055575667)) ;
#5843 = CARTESIAN_POINT('Ctrl Pts',(29.5755892637938,53.2664641483663,72.758575460154)) ;
#5844 = CARTESIAN_POINT('Ctrl Pts',(29.484238140167,53.5254861983917,72.8803269249872)) ;
#5845 = CARTESIAN_POINT('Ctrl Pts',(29.4093245268927,53.7311956119235,72.9753597322604)) ;
#5846 = CARTESIAN_POINT('Ctrl Pts',(29.3079124503544,54.0017837515365,73.0978749780937)) ;
#5847 = CARTESIAN_POINT('Ctrl Pts',(29.283425087555,54.0665473332678,73.1270096919038)) ;
#5848 = CARTESIAN_POINT('Ctrl Pts',(29.1845494593619,54.3258257235604,73.242870772065)) ;
#5849 = CARTESIAN_POINT('Ctrl Pts',(29.1083294283321,54.5205088505458,73.3282083519262)) ;
#5850 = CARTESIAN_POINT('Ctrl Pts',(28.9995814541329,54.791419972509,73.4445685151767)) ;
#5851 = CARTESIAN_POINT('Ctrl Pts',(28.9686820524854,54.8676682916987,73.4770501086411)) ;
#5852 = CARTESIAN_POINT('Ctrl Pts',(28.8267551920768,55.2146576988594,73.6236213185704)) ;
#5853 = CARTESIAN_POINT('Ctrl Pts',(28.7126177925182,55.4852678000175,73.7343097498549)) ;
#5854 = CARTESIAN_POINT('Ctrl Pts',(28.5205593627065,55.9272948494755,73.9092265825147)) ;
#5855 = CARTESIAN_POINT('Ctrl Pts',(28.4446562120935,56.0987899530306,73.9756393685776)) ;
#5856 = CARTESIAN_POINT('Ctrl Pts',(28.3229756917417,56.3691923043808,74.0779062132529)) ;
#5857 = CARTESIAN_POINT('Ctrl Pts',(28.2780539678421,56.4680781862301,74.1147900724143)) ;
#5858 = CARTESIAN_POINT('Ctrl Pts',(28.0405709787764,56.9862401445908,74.3052598553338)) ;
#5859 = CARTESIAN_POINT('Ctrl Pts',(27.8407773809973,57.405632674829,74.4501409788345)) ;
#5860 = CARTESIAN_POINT('Ctrl Pts',(27.6341058620046,57.8256477521656,74.5851509282983)) ;
#5861 = CARTESIAN_POINT('',(27.6340702364062,57.8265499696741,74.5851752834194)) ;
#5862 = CARTESIAN_POINT('Ctrl Pts',(27.6340835637164,57.8256930685524,74.5851654947913)) ;
#5863 = CARTESIAN_POINT('Ctrl Pts',(27.634069752068,57.8259720706221,74.5851745186134)) ;
#5864 = CARTESIAN_POINT('Ctrl Pts',(27.6340698179607,57.8262610184418,74.5851746396025)) ;
#5865 = CARTESIAN_POINT('Ctrl Pts',(27.6340699848282,57.826549969134,74.5851749064526)) ;
#5866 = CARTESIAN_POINT('',(27.6340703658488,58.7660385728177,74.5851754951966)) ;
#5867 = CARTESIAN_POINT('',(27.6340704790844,43.8830586252741,74.5851756661337)) ;
#5868 = CARTESIAN_POINT('Ctrl Pts',(27.6340702509209,58.766038570856,74.5851753253735)) ;
#5869 = CARTESIAN_POINT('Ctrl Pts',(27.7600299425795,58.5098890074295,74.5028909240232)) ;
#5870 = CARTESIAN_POINT('Ctrl Pts',(27.8836766516442,58.253780180156,74.4167771302412)) ;
#5871 = CARTESIAN_POINT('Ctrl Pts',(28.0101438591921,57.9857873917738,74.3229987438209)) ;
#5872 = CARTESIAN_POINT('Ctrl Pts',(28.0157801192334,57.973831995724,74.318807191727)) ;
#5873 = CARTESIAN_POINT('Ctrl Pts',(28.147615118801,57.6939113334552,74.2204803220524)) ;
#5874 = CARTESIAN_POINT('Ctrl Pts',(28.2708796194584,57.426263839475,74.1224374801235)) ;
#5875 = CARTESIAN_POINT('Ctrl Pts',(28.3922280683633,57.1556222836718,74.0196140263438)) ;
#5876 = CARTESIAN_POINT('Ctrl Pts',(28.3935945166274,57.1525737751886,74.0184553483433)) ;
#5877 = CARTESIAN_POINT('Ctrl Pts',(28.5215787684715,56.8669561800162,73.9098533842011)) ;
#5878 = CARTESIAN_POINT('Ctrl Pts',(28.644551100692,56.5844497694098,73.7983737701696)) ;
#5879 = CARTESIAN_POINT('Ctrl Pts',(28.8692587681259,56.0525625568707,73.5808364497842)) ;
#5880 = CARTESIAN_POINT('Ctrl Pts',(28.9716456686909,55.8030380923874,73.4758091882058)) ;
#5881 = CARTESIAN_POINT('Ctrl Pts',(29.0840928441225,55.5203596436975,73.3535741415821)) ;
#5882 = CARTESIAN_POINT('Ctrl Pts',(29.0971736066216,55.487339023581,73.3392450682227)) ;
#5883 = CARTESIAN_POINT('Ctrl Pts',(29.202780837364,55.2196257773339,73.2226665271722)) ;
#5884 = CARTESIAN_POINT('Ctrl Pts',(29.2927320594827,54.9847737061719,73.1177666619654)) ;
#5885 = CARTESIAN_POINT('Ctrl Pts',(29.3975387478343,54.7017289710564,72.9885809457978)) ;
#5886 = CARTESIAN_POINT('Ctrl Pts',(29.4152135223729,54.6536565138857,72.9665446527025)) ;
#5887 = CARTESIAN_POINT('Ctrl Pts',(29.5130363251233,54.3856593021878,72.8431766243648)) ;
#5888 = CARTESIAN_POINT('Ctrl Pts',(29.5906542386682,54.1659530442002,72.7399905215469)) ;
#5889 = CARTESIAN_POINT('Ctrl Pts',(29.6871182370823,53.8833573751818,72.6047103924036)) ;
#5890 = CARTESIAN_POINT('Ctrl Pts',(29.7083973107427,53.8203770818542,72.5744025927511)) ;
#5891 = CARTESIAN_POINT('Ctrl Pts',(29.7978525182514,53.5528374916877,72.4449910678865)) ;
#5892 = CARTESIAN_POINT('Ctrl Pts',(29.8638327717365,53.348275131605,72.3445230657125)) ;
#5893 = CARTESIAN_POINT('Ctrl Pts',(29.9516247240262,53.0657839416432,72.2036705749113)) ;
#5894 = CARTESIAN_POINT('Ctrl Pts',(29.9754972013003,52.9878441570689,72.1645872031147)) ;
#5895 = CARTESIAN_POINT('Ctrl Pts',(30.0562338081894,52.7203373164194,72.029683143324)) ;
#5896 = CARTESIAN_POINT('Ctrl Pts',(30.1113680689016,52.5307715920929,71.932783916218)) ;
#5897 = CARTESIAN_POINT('Ctrl Pts',(30.1903188679312,52.2481729096978,71.7866399275519)) ;
#5898 = CARTESIAN_POINT('Ctrl Pts',(30.2157706265884,52.1552026240065,71.7382875582465)) ;
#5899 = CARTESIAN_POINT('Ctrl Pts',(30.2785909073748,51.9208262076072,71.6157534900977)) ;
#5900 = CARTESIAN_POINT('Ctrl Pts',(30.3152863743369,51.7794006203881,71.5411932918103)) ;
#5901 = CARTESIAN_POINT('Ctrl Pts',(30.3591587242532,51.60452330737,71.448227653069)) ;
#5902 = CARTESIAN_POINT('Ctrl Pts',(30.3674716743981,51.5711185095033,71.4304337880207)) ;
#5903 = CARTESIAN_POINT('Ctrl Pts',(30.4023942104701,51.4296212255096,71.3549201756335)) ;
#5904 = CARTESIAN_POINT('Ctrl Pts',(30.4283592597888,51.3215155544796,71.2968765915474)) ;
#5905 = CARTESIAN_POINT('Ctrl Pts',(30.4908183940924,51.0537368175205,71.152420071463)) ;
#5906 = CARTESIAN_POINT('Ctrl Pts',(30.5264364258323,50.8941113379638,71.0656618252809)) ;
#5907 = CARTESIAN_POINT('Ctrl Pts',(30.5865621606833,50.6118990016945,70.9111362808276)) ;
#5908 = CARTESIAN_POINT('Ctrl Pts',(30.6117380024369,50.4892574041004,70.8436019858225)) ;
#5909 = CARTESIAN_POINT('Ctrl Pts',(30.6644649877661,50.2223202255289,70.6957801754687)) ;
#5910 = CARTESIAN_POINT('Ctrl Pts',(30.6916211845518,50.0780242815205,70.6154142118301)) ;
#5911 = CARTESIAN_POINT('Ctrl Pts',(30.7419452106475,49.7965776405067,70.4578470852657)) ;
#5912 = CARTESIAN_POINT('Ctrl Pts',(30.7652403570727,49.6594152246682,70.3806899793754)) ;
#5913 = CARTESIAN_POINT('Ctrl Pts',(30.8081006160294,49.3929482765754,70.2301253928115)) ;
#5914 = CARTESIAN_POINT('Ctrl Pts',(30.8278110118762,49.2636615036751,70.1567171260021)) ;
#5915 = CARTESIAN_POINT('Ctrl Pts',(30.8682544166326,48.9827045772249,69.9965436405729)) ;
#5916 = CARTESIAN_POINT('Ctrl Pts',(30.8885647864592,48.8310367404956,69.9096944982135)) ;
#5917 = CARTESIAN_POINT('Ctrl Pts',(30.9214998312479,48.5648138959559,69.7567724669571)) ;
#5918 = CARTESIAN_POINT('Ctrl Pts',(30.9347940974624,48.4502757510319,69.6908019636932)) ;
#5919 = CARTESIAN_POINT('Ctrl Pts',(30.9652388398132,48.169433296079,69.528627660098)) ;
#5920 = CARTESIAN_POINT('Ctrl Pts',(30.9814192229612,48.0031363324805,69.4322203252873)) ;
#5921 = CARTESIAN_POINT('Ctrl Pts',(31.0043480443608,47.7369180822766,69.2773466723917)) ;
#5922 = CARTESIAN_POINT('Ctrl Pts',(31.0122778434617,47.6369794599077,69.2191365361054)) ;
#5923 = CARTESIAN_POINT('Ctrl Pts',(31.032663409965,47.3560315968962,69.0553072016704)) ;
#5924 = CARTESIAN_POINT('Ctrl Pts',(31.0435800890746,47.1749633576186,68.9494892744708)) ;
#5925 = CARTESIAN_POINT('Ctrl Pts',(31.0657783101076,46.7126338479033,68.6787096511655)) ;
#5926 = CARTESIAN_POINT('Ctrl Pts',(31.0739241994752,46.4312682182311,68.513324772655)) ;
#5927 = CARTESIAN_POINT('Ctrl Pts',(31.0773432634457,46.0783306369255,68.3060020525323)) ;
#5928 = CARTESIAN_POINT('Ctrl Pts',(31.0776880663112,46.0072326116127,68.2642279969038)) ;
#5929 = CARTESIAN_POINT('Ctrl Pts',(31.0776881068351,45.9361079682071,68.2224337399966)) ;
#5930 = CARTESIAN_POINT('',(15.8776875119243,53.1208403600521,68.2224337443077)) ;
#5931 = CARTESIAN_POINT('',(16.3751686437571,57.8256698856438,65.5179563592932)) ;
#5932 = CARTESIAN_POINT('Ctrl Pts',(15.8776875119243,53.1208403600521,68.2224337443077)) ;
#5933 = CARTESIAN_POINT('Ctrl Pts',(15.8776877387063,53.1871490007968,68.1834760773303)) ;
#5934 = CARTESIAN_POINT('Ctrl Pts',(15.8779875469879,53.2534600732653,68.1445152562114)) ;
#5935 = CARTESIAN_POINT('Ctrl Pts',(15.8810308727502,53.5902066966755,67.946652756444)) ;
#5936 = CARTESIAN_POINT('Ctrl Pts',(15.888467388127,53.860642481361,67.7876705864655)) ;
#5937 = CARTESIAN_POINT('Ctrl Pts',(15.9034088077128,54.1864226824151,67.5968601517276)) ;
#5938 = CARTESIAN_POINT('Ctrl Pts',(15.9061431888012,54.2415348490089,67.5645950586243)) ;
#5939 = CARTESIAN_POINT('Ctrl Pts',(15.9195506920211,54.4928052763559,67.4175674694017)) ;
#5940 = CARTESIAN_POINT('Ctrl Pts',(15.9326424619461,54.6891498815712,67.3028817310846)) ;
#5941 = CARTESIAN_POINT('Ctrl Pts',(15.9498927681818,54.9048361953365,67.1772400978473)) ;
#5942 = CARTESIAN_POINT('Ctrl Pts',(15.9514802349652,54.9243619105753,67.1658693825961)) ;
#5943 = CARTESIAN_POINT('Ctrl Pts',(15.9676855587794,55.1204950653914,67.0516873615927)) ;
#5944 = CARTESIAN_POINT('Ctrl Pts',(15.9843658342187,55.2970548144963,66.9492903649222)) ;
#5945 = CARTESIAN_POINT('Ctrl Pts',(16.0131302290761,55.5676362557331,66.7929442727957)) ;
#5946 = CARTESIAN_POINT('Ctrl Pts',(16.0237231107349,55.6616980715273,66.738701338355)) ;
#5947 = CARTESIAN_POINT('Ctrl Pts',(16.0670697461354,56.0262039248394,66.5289163363484)) ;
#5948 = CARTESIAN_POINT('Ctrl Pts',(16.1041291773361,56.2965161322938,66.3742241105852)) ;
#5949 = CARTESIAN_POINT('Ctrl Pts',(16.2108439844322,56.9862189711356,65.9833159733028)) ;
#5950 = CARTESIAN_POINT('Ctrl Pts',(16.2873230212551,57.4056466389749,65.7486646609522)) ;
#5951 = CARTESIAN_POINT('Ctrl Pts',(16.3751640146366,57.8256477521648,65.5179685166535)) ;
#5952 = CARTESIAN_POINT('',(16.3751780994845,57.8271591849708,65.5179277057667)) ;
#5953 = CARTESIAN_POINT('Ctrl Pts',(16.3751735099526,57.8256931526636,65.5179435793076)) ;
#5954 = CARTESIAN_POINT('Ctrl Pts',(16.375179360142,57.8261752208488,65.5179282095724)) ;
#5955 = CARTESIAN_POINT('Ctrl Pts',(16.3751789637411,57.8266672012913,65.5179280439107)) ;
#5956 = CARTESIAN_POINT('Ctrl Pts',(16.3751780994845,57.8271591849708,65.5179277057666)) ;
#5957 = CARTESIAN_POINT('',(16.3751775163941,58.7660404020332,65.5179292370655)) ;
#5958 = CARTESIAN_POINT('',(16.3751780994845,43.8830586252741,65.5179277057667)) ;
#5959 = CARTESIAN_POINT('',(15.87768801576,54.0610773150226,68.2224337400137)) ;
#5960 = CARTESIAN_POINT('Ctrl Pts',(16.3751775163941,58.7660404020332,65.5179292370655)) ;
#5961 = CARTESIAN_POINT('Ctrl Pts',(16.318048692533,58.4927517118959,65.6679597032189)) ;
#5962 = CARTESIAN_POINT('Ctrl Pts',(16.2656591635554,58.2194425159302,65.8198505460739)) ;
#5963 = CARTESIAN_POINT('Ctrl Pts',(16.1974167526078,57.8271113937991,66.0401048199781)) ;
#5964 = CARTESIAN_POINT('Ctrl Pts',(16.1776103066955,57.7079337985678,66.1073050755783)) ;
#5965 = CARTESIAN_POINT('Ctrl Pts',(16.1031323071922,57.2377082464182,66.3735075476004)) ;
#5966 = CARTESIAN_POINT('Ctrl Pts',(16.0556887898407,56.8868665748457,66.574271919069)) ;
#5967 = CARTESIAN_POINT('Ctrl Pts',(16.0118950098979,56.495184630307,66.8002830769449)) ;
#5968 = CARTESIAN_POINT('Ctrl Pts',(16.0074344951922,56.4542916276441,66.8239023131688)) ;
#5969 = CARTESIAN_POINT('Ctrl Pts',(15.9614349400052,56.0217278514861,67.0739792638625)) ;
#5970 = CARTESIAN_POINT('Ctrl Pts',(15.9300813885958,55.6299821269397,67.3022360334898)) ;
#5971 = CARTESIAN_POINT('Ctrl Pts',(15.8992014526108,55.05188349398,67.6406353482144)) ;
#5972 = CARTESIAN_POINT('Ctrl Pts',(15.8916062131826,54.8657705646704,67.7498652264096)) ;
#5973 = CARTESIAN_POINT('Ctrl Pts',(15.8860940383579,54.6695659260189,67.865031687881)) ;
#5974 = CARTESIAN_POINT('Ctrl Pts',(15.8858167980585,54.6594490920002,67.8709700152553)) ;
#5975 = CARTESIAN_POINT('Ctrl Pts',(15.8803052730986,54.4531311678522,67.9920733247475)) ;
#5976 = CARTESIAN_POINT('Ctrl Pts',(15.8776880157599,54.2570462500708,68.1072484844461)) ;
#5977 = CARTESIAN_POINT('Ctrl Pts',(15.87768801576,54.0610773150155,68.2224337400016)) ;
#5978 = CARTESIAN_POINT('',(17.5258214371218,45.3830586252742,72.9484557858036)) ;
#5979 = CARTESIAN_POINT('Ctrl Pts',(15.87768801576,54.0610773150297,68.2224337400258)) ;
#5980 = CARTESIAN_POINT('Ctrl Pts',(15.8776880157602,53.9598262897505,68.2819463623541)) ;
#5981 = CARTESIAN_POINT('Ctrl Pts',(15.8783870294523,53.8586011420046,68.3414526422372)) ;
#5982 = CARTESIAN_POINT('Ctrl Pts',(15.8797847080111,53.7573959543402,68.4009423563146)) ;
#5983 = CARTESIAN_POINT('Ctrl Pts',(15.8834278383639,53.4935987538091,68.5560057517411)) ;
#5984 = CARTESIAN_POINT('Ctrl Pts',(15.8918090487111,53.2298184766074,68.7107644985098)) ;
#5985 = CARTESIAN_POINT('Ctrl Pts',(15.9049188360724,52.966059183431,68.8652143800119)) ;
#5986 = CARTESIAN_POINT('Ctrl Pts',(15.9058492786295,52.947339362548,68.8761761705229)) ;
#5987 = CARTESIAN_POINT('Ctrl Pts',(15.9068035616431,52.9286196473653,68.8871364041267)) ;
#5988 = CARTESIAN_POINT('Ctrl Pts',(15.9077816916672,52.9099000393348,68.8980950785868)) ;
#5989 = CARTESIAN_POINT('Ctrl Pts',(15.922541707333,52.6274205110582,69.063461852667)) ;
#5990 = CARTESIAN_POINT('Ctrl Pts',(15.9427340901668,52.3449496227476,69.2284477477508)) ;
#5991 = CARTESIAN_POINT('Ctrl Pts',(15.9683106417657,52.0622051908031,69.3925839247815)) ;
#5992 = CARTESIAN_POINT('Ctrl Pts',(15.9735819620023,52.0039316412923,69.4264123456382)) ;
#5993 = CARTESIAN_POINT('Ctrl Pts',(15.9790825849275,51.9456496648422,69.4602098098499)) ;
#5994 = CARTESIAN_POINT('Ctrl Pts',(15.984812754553,51.8873592927888,69.4939762363384)) ;
#5995 = CARTESIAN_POINT('Ctrl Pts',(15.992984279923,51.8042341350373,69.542128948865)) ;
#5996 = CARTESIAN_POINT('Ctrl Pts',(16.0016230688955,51.7210878853372,69.590221238424)) ;
#5997 = CARTESIAN_POINT('Ctrl Pts',(16.0107299125882,51.6379247117809,69.6382503543534)) ;
#5998 = CARTESIAN_POINT('Ctrl Pts',(16.0214869739339,51.5396918453961,69.6949826497423)) ;
#5999 = CARTESIAN_POINT('Ctrl Pts',(16.0329010704352,51.4414217778531,69.7516433072497)) ;
#6000 = CARTESIAN_POINT('Ctrl Pts',(16.0449492807277,51.3432074537042,69.8081181022716)) ;
#6001 = CARTESIAN_POINT('Ctrl Pts',(16.0502540143438,51.2999644479586,69.8329835168309)) ;
#6002 = CARTESIAN_POINT('Ctrl Pts',(16.0556820779081,51.2567285488362,69.8578153874229)) ;
#6003 = CARTESIAN_POINT('Ctrl Pts',(16.061231033401,51.2135073972261,69.8826041616199)) ;
#6004 = CARTESIAN_POINT('Ctrl Pts',(16.0789544785872,51.0754584054067,69.9617798697825)) ;
#6005 = CARTESIAN_POINT('Ctrl Pts',(16.0979255370188,50.9375082770569,70.0405823222603)) ;
#6006 = CARTESIAN_POINT('Ctrl Pts',(16.1181351551565,50.7996661916347,70.1190047753123)) ;
#6007 = CARTESIAN_POINT('Ctrl Pts',(16.1393118540383,50.6552280178723,70.2011799387692)) ;
#6008 = CARTESIAN_POINT('Ctrl Pts',(16.1618492668502,50.5109057227833,70.2829413721308)) ;
#6009 = CARTESIAN_POINT('Ctrl Pts',(16.1857433083364,50.3666994632668,70.3642886332832)) ;
#6010 = CARTESIAN_POINT('Ctrl Pts',(16.2217335002578,50.1494900406054,70.4868172370292)) ;
#6011 = CARTESIAN_POINT('Ctrl Pts',(16.2607672253128,49.9324691220747,70.6082868352782)) ;
#6012 = CARTESIAN_POINT('Ctrl Pts',(16.3027912912963,49.715573436112,70.7285975401703)) ;
#6013 = CARTESIAN_POINT('Ctrl Pts',(16.3152762507575,49.65113574349,70.7643407325098)) ;
#6014 = CARTESIAN_POINT('Ctrl Pts',(16.3280255475019,49.5867095881029,70.7999827452736)) ;
#6015 = CARTESIAN_POINT('Ctrl Pts',(16.3410378746391,49.5222932712664,70.8355209492688)) ;
#6016 = CARTESIAN_POINT('Ctrl Pts',(16.3926299094743,49.2668916949656,70.9764248966691)) ;
#6017 = CARTESIAN_POINT('Ctrl Pts',(16.4484105732616,49.0117332177746,71.1158311082438)) ;
#6018 = CARTESIAN_POINT('Ctrl Pts',(16.5082176847315,48.7565688872915,71.2533549374115)) ;
#6019 = CARTESIAN_POINT('Ctrl Pts',(16.5142510416214,48.730827843567,71.2672283769047)) ;
#6020 = CARTESIAN_POINT('Ctrl Pts',(16.5203253348275,48.7050867402745,71.2810826771504)) ;
#6021 = CARTESIAN_POINT('Ctrl Pts',(16.5264403710249,48.6793453218294,71.2949174554279)) ;
#6022 = CARTESIAN_POINT('Ctrl Pts',(16.5931574897773,48.3984977167074,71.445859578331)) ;
#6023 = CARTESIAN_POINT('Ctrl Pts',(16.6647653754236,48.1176791006564,71.5945788691957)) ;
#6024 = CARTESIAN_POINT('Ctrl Pts',(16.7412285650833,47.8368320972583,71.7409723669579)) ;
#6025 = CARTESIAN_POINT('Ctrl Pts',(16.7670315043542,47.7420586748396,71.7903736873739)) ;
#6026 = CARTESIAN_POINT('Ctrl Pts',(16.7933718109271,47.6472611060918,71.8394797343875)) ;
#6027 = CARTESIAN_POINT('Ctrl Pts',(16.820248904836,47.5524394572103,71.8882903226211)) ;
#6028 = CARTESIAN_POINT('Ctrl Pts',(16.8730041029354,47.366320567728,71.9840972673871)) ;
#6029 = CARTESIAN_POINT('Ctrl Pts',(16.9278282648647,47.1801103309901,72.078769184525)) ;
#6030 = CARTESIAN_POINT('Ctrl Pts',(16.9847270270042,46.9938102819949,72.1723017882395)) ;
#6031 = CARTESIAN_POINT('Ctrl Pts',(17.0380761434748,46.8191326152305,72.2599993335239)) ;
#6032 = CARTESIAN_POINT('Ctrl Pts',(17.0932559186719,46.6443819715505,72.346703095831)) ;
#6033 = CARTESIAN_POINT('Ctrl Pts',(17.1502082429138,46.4694842601059,72.4323030638899)) ;
#6034 = CARTESIAN_POINT('Ctrl Pts',(17.1849311118386,46.3628520832706,72.4844919167672)) ;
#6035 = CARTESIAN_POINT('Ctrl Pts',(17.220311010757,46.2561640031219,72.5362680765448)) ;
#6036 = CARTESIAN_POINT('Ctrl Pts',(17.2563345933752,46.1494043647081,72.5876097494857)) ;
#6037 = CARTESIAN_POINT('Ctrl Pts',(17.3424138503274,45.8942995228455,72.7102919686384)) ;
#6038 = CARTESIAN_POINT('Ctrl Pts',(17.4322561663653,45.6388798336617,72.8306213626458)) ;
#6039 = CARTESIAN_POINT('Ctrl Pts',(17.5258214447123,45.3830586252743,72.9484557797765)) ;
#6040 = CARTESIAN_POINT('',(17.1981488755629,45.3830634197606,72.5034839444725)) ;
#6041 = CARTESIAN_POINT('Origin',(23.47768801576,45.3830586252741,68.2224337400009)) ;
#6042 = CARTESIAN_POINT('Ctrl Pts',(17.1981485126538,45.3830652730852,72.5034835325328)) ;
#6043 = CARTESIAN_POINT('Ctrl Pts',(17.1284537177608,45.5935267173151,72.4012543694107)) ;
#6044 = CARTESIAN_POINT('Ctrl Pts',(17.0613339404697,45.8038970071019,72.2974387949214)) ;
#6045 = CARTESIAN_POINT('Ctrl Pts',(16.962354850366,46.1264421086301,72.1358443111681)) ;
#6046 = CARTESIAN_POINT('Ctrl Pts',(16.9286362979452,46.2386508709495,72.0791500238972)) ;
#6047 = CARTESIAN_POINT('Ctrl Pts',(16.8491643584742,46.5090378891581,71.9414799227803)) ;
#6048 = CARTESIAN_POINT('Ctrl Pts',(16.8041447292678,46.6672026152944,71.8600789986582)) ;
#6049 = CARTESIAN_POINT('Ctrl Pts',(16.7155010485011,46.9896373648865,71.6926127002568)) ;
#6050 = CARTESIAN_POINT('Ctrl Pts',(16.671982425607,47.1538972164843,71.606471066007)) ;
#6051 = CARTESIAN_POINT('Ctrl Pts',(16.602990660836,47.4245379703279,71.4631823632395)) ;
#6052 = CARTESIAN_POINT('Ctrl Pts',(16.5765640699983,47.5309048058355,71.4065194705275)) ;
#6053 = CARTESIAN_POINT('Ctrl Pts',(16.4984989659946,47.8535340062433,71.2335950304104)) ;
#6054 = CARTESIAN_POINT('Ctrl Pts',(16.4490923792239,48.069949799947,71.1163855119266)) ;
#6055 = CARTESIAN_POINT('Ctrl Pts',(16.3909875905432,48.3407265621182,70.9682854354735)) ;
#6056 = CARTESIAN_POINT('Ctrl Pts',(16.3794669871731,48.3952944415037,70.93836556585)) ;
#6057 = CARTESIAN_POINT('Ctrl Pts',(16.3125132413207,48.7177229150411,70.7611427633822)) ;
#6058 = CARTESIAN_POINT('Ctrl Pts',(16.261446163163,48.9853758417281,70.6121169893423)) ;
#6059 = CARTESIAN_POINT('Ctrl Pts',(16.2146236633515,49.2558099187254,70.4602672618887)) ;
#6060 = CARTESIAN_POINT('Ctrl Pts',(16.214142876459,49.2585897556055,70.4587062362067)) ;
#6061 = CARTESIAN_POINT('Ctrl Pts',(16.2136625986088,49.2613695957061,70.4571450723729)) ;
#6062 = CARTESIAN_POINT('Ctrl Pts',(16.1669395803816,49.5318016375275,70.3052698896535)) ;
#6063 = CARTESIAN_POINT('Ctrl Pts',(16.1249977580323,49.8022075449293,70.1520021909819)) ;
#6064 = CARTESIAN_POINT('Ctrl Pts',(16.0811359667075,50.1215492476701,69.9693871962945)) ;
#6065 = CARTESIAN_POINT('Ctrl Pts',(16.0745730607129,50.1705005823631,69.9413635189957)) ;
#6066 = CARTESIAN_POINT('Ctrl Pts',(16.0391975693541,50.4409777252529,69.7863498226791)) ;
#6067 = CARTESIAN_POINT('Ctrl Pts',(16.0135016772283,50.6626055143604,69.6587142024686)) ;
#6068 = CARTESIAN_POINT('Ctrl Pts',(15.9808848681758,50.9851624100752,69.4720136822115)) ;
#6069 = CARTESIAN_POINT('Ctrl Pts',(15.9713682691362,51.0859939056647,69.4135045221654)) ;
#6070 = CARTESIAN_POINT('Ctrl Pts',(15.9476364035747,51.3568997827781,69.2560008379473)) ;
#6071 = CARTESIAN_POINT('Ctrl Pts',(15.9346854871418,51.5269679364528,69.1568228822683)) ;
#6072 = CARTESIAN_POINT('Ctrl Pts',(15.9138635938771,51.8494753760342,68.9684861773292)) ;
#6073 = CARTESIAN_POINT('Ctrl Pts',(15.9055941627483,52.0019638251988,68.879264954564)) ;
#6074 = CARTESIAN_POINT('Ctrl Pts',(15.8937230547787,52.2724926312743,68.7207266752105)) ;
#6075 = CARTESIAN_POINT('Ctrl Pts',(15.8894894402357,52.3905429898142,68.6514552394551)) ;
#6076 = CARTESIAN_POINT('Ctrl Pts',(15.8805247574606,52.7126477889991,68.4622522192294)) ;
#6077 = CARTESIAN_POINT('Ctrl Pts',(15.8776868138709,52.9167369537098,68.342348621825)) ;
#6078 = CARTESIAN_POINT('Ctrl Pts',(15.8776875119243,53.1208403600521,68.2224337443077)) ;
#6079 = CARTESIAN_POINT('',(26.0416037428036,45.3830634900494,61.0679708775511)) ;
#6080 = CARTESIAN_POINT('',(30.8133987679008,57.8256696110844,66.2356456049943)) ;
#6081 = CARTESIAN_POINT('Ctrl Pts',(26.041604258221,45.3830652730984,61.0679709929564)) ;
#6082 = CARTESIAN_POINT('Ctrl Pts',(26.1580773630691,45.593526784071,61.1097105638754)) ;
#6083 = CARTESIAN_POINT('Ctrl Pts',(26.2734067453744,45.8038922450035,61.1542499492565)) ;
#6084 = CARTESIAN_POINT('Ctrl Pts',(26.4141578631216,46.0632318316992,61.212585328639)) ;
#6085 = CARTESIAN_POINT('Ctrl Pts',(26.4407101196587,46.1122612415126,61.2237676201864)) ;
#6086 = CARTESIAN_POINT('Ctrl Pts',(26.586832843751,46.3827042839367,61.2862869523435)) ;
#6087 = CARTESIAN_POINT('Ctrl Pts',(26.7052078067137,46.604012592347,61.3405705010222)) ;
#6088 = CARTESIAN_POINT('Ctrl Pts',(26.8420129650536,46.8632622432158,61.4076107275278)) ;
#6089 = CARTESIAN_POINT('Ctrl Pts',(26.8619485618899,46.9011261856477,61.4174887031528)) ;
#6090 = CARTESIAN_POINT('Ctrl Pts',(27.0040850331528,47.1717033808736,61.4886953286622)) ;
#6091 = CARTESIAN_POINT('Ctrl Pts',(27.1246612717725,47.4044689603647,61.5532259360897)) ;
#6092 = CARTESIAN_POINT('Ctrl Pts',(27.257162671145,47.6638628919003,61.6288144342943)) ;
#6093 = CARTESIAN_POINT('Ctrl Pts',(27.2707127104083,47.6904386808345,61.6365999303412)) ;
#6094 = CARTESIAN_POINT('Ctrl Pts',(27.408558191849,47.961299863614,61.7163691635019)) ;
#6095 = CARTESIAN_POINT('Ctrl Pts',(27.5307957603664,48.2057236046437,61.7918123691392)) ;
#6096 = CARTESIAN_POINT('Ctrl Pts',(27.6581094410944,48.4649882125096,61.8754536832722)) ;
#6097 = CARTESIAN_POINT('Ctrl Pts',(27.6655357210229,48.4801277704428,61.8803512377111)) ;
#6098 = CARTESIAN_POINT('Ctrl Pts',(27.7981505933644,48.7507815722807,61.9681441307179)) ;
#6099 = CARTESIAN_POINT('Ctrl Pts',(27.9209138440538,49.0060603871173,62.0547560051701)) ;
#6100 = CARTESIAN_POINT('Ctrl Pts',(28.0426272365086,49.2650911286676,62.1461408986514)) ;
#6101 = CARTESIAN_POINT('Ctrl Pts',(28.0443755667558,49.2688131587718,62.147454760076)) ;
#6102 = CARTESIAN_POINT('Ctrl Pts',(28.1677560109025,49.5315653220715,62.2402578391401)) ;
#6103 = CARTESIAN_POINT('Ctrl Pts',(28.2865807178825,49.7905771610405,62.3353500873029)) ;
#6104 = CARTESIAN_POINT('Ctrl Pts',(28.4060264763688,50.0572510953393,62.4369777978504)) ;
#6105 = CARTESIAN_POINT('Ctrl Pts',(28.4094629600844,50.0649289262853,62.4399069315551)) ;
#6106 = CARTESIAN_POINT('Ctrl Pts',(28.5253015441136,50.3239244418434,62.538821762771)) ;
#6107 = CARTESIAN_POINT('Ctrl Pts',(28.634827348025,50.5754015948757,62.6380105542769)) ;
#6108 = CARTESIAN_POINT('Ctrl Pts',(28.749572034541,50.8461423400794,62.7481881019863)) ;
#6109 = CARTESIAN_POINT('Ctrl Pts',(28.7576536046867,50.8652509230882,62.7559824719168)) ;
#6110 = CARTESIAN_POINT('Ctrl Pts',(28.8671091242344,51.1245997230133,62.8620169997531)) ;
#6111 = CARTESIAN_POINT('Ctrl Pts',(28.9659486623374,51.3650618940756,62.9632623213938)) ;
#6112 = CARTESIAN_POINT('Ctrl Pts',(29.0738923449893,51.6358437425653,63.0801758596971)) ;
#6113 = CARTESIAN_POINT('Ctrl Pts',(29.0860186098835,51.6663832990628,63.0934036352977)) ;
#6114 = CARTESIAN_POINT('Ctrl Pts',(29.2051570782229,51.9676379850836,63.2242945123136)) ;
#6115 = CARTESIAN_POINT('Ctrl Pts',(29.308462676244,52.2381644564847,63.34520603459)) ;
#6116 = CARTESIAN_POINT('Ctrl Pts',(29.4877453362116,52.7256472364854,63.568885979738)) ;
#6117 = CARTESIAN_POINT('Ctrl Pts',(29.5649977360443,52.9427458529092,63.6704069597754)) ;
#6118 = CARTESIAN_POINT('Ctrl Pts',(29.6579933638176,53.2131562545837,63.7992211617736)) ;
#6119 = CARTESIAN_POINT('Ctrl Pts',(29.6761702732096,53.2664641483689,63.8247299027501)) ;
#6120 = CARTESIAN_POINT('Ctrl Pts',(29.7637337475682,53.5254861983816,63.9492332558931)) ;
#6121 = CARTESIAN_POINT('Ctrl Pts',(29.830965738571,53.7311956119134,64.0498470884217)) ;
#6122 = CARTESIAN_POINT('Ctrl Pts',(29.9161466063752,54.0017837515308,64.1841549976686)) ;
#6123 = CARTESIAN_POINT('Ctrl Pts',(29.9362883545417,54.0665473332625,64.2164469853188)) ;
#6124 = CARTESIAN_POINT('Ctrl Pts',(30.0159245403778,54.325825723567,64.3462863385794)) ;
#6125 = CARTESIAN_POINT('Ctrl Pts',(30.0735321168821,54.5205088505445,64.445146658184)) ;
#6126 = CARTESIAN_POINT('Ctrl Pts',(30.1505922362448,54.7914199725069,64.5845293955896)) ;
#6127 = CARTESIAN_POINT('Ctrl Pts',(30.1719356271454,54.8676682916929,64.6239538372645)) ;
#6128 = CARTESIAN_POINT('Ctrl Pts',(30.2674753196619,55.2146576988569,64.8042272975172)) ;
#6129 = CARTESIAN_POINT('Ctrl Pts',(30.3374758773342,55.4852678000175,64.9469830214306)) ;
#6130 = CARTESIAN_POINT('Ctrl Pts',(30.4444823520982,55.9272948494787,65.1836937164577)) ;
#6131 = CARTESIAN_POINT('Ctrl Pts',(30.4841893015841,56.0987899530359,65.2764045819959)) ;
#6132 = CARTESIAN_POINT('Ctrl Pts',(30.5438495019435,56.3691923043857,65.4237318267551)) ;
#6133 = CARTESIAN_POINT('Ctrl Pts',(30.565046560445,56.4680781862336,65.4778526642952)) ;
#6134 = CARTESIAN_POINT('Ctrl Pts',(30.6728078091545,56.9862401445904,65.7625708083994)) ;
#6135 = CARTESIAN_POINT('Ctrl Pts',(30.7488583286256,57.4056326749329,65.9973565406346)) ;
#6136 = CARTESIAN_POINT('Ctrl Pts',(30.8133954092186,57.8256477522358,66.2356332043538)) ;
#6137 = CARTESIAN_POINT('',(30.8134080024022,57.8271591829153,66.2356745000382)) ;
#6138 = CARTESIAN_POINT('Ctrl Pts',(30.8134023722464,57.8256930687507,66.2356589126527)) ;
#6139 = CARTESIAN_POINT('Ctrl Pts',(30.8134066863751,57.8261751443407,66.2356748334161)) ;
#6140 = CARTESIAN_POINT('Ctrl Pts',(30.8134071043806,57.8266671620021,66.2356747344862)) ;
#6141 = CARTESIAN_POINT('Ctrl Pts',(30.8134080024022,57.8271591829153,66.2356745000382)) ;
#6142 = CARTESIAN_POINT('',(30.8134078048396,58.7660385728356,66.2356745549092)) ;
#6143 = CARTESIAN_POINT('',(30.8134080024022,43.8830586252741,66.2356745000382)) ;
#6144 = CARTESIAN_POINT('',(25.5149631655986,45.3830586252742,60.9005821906198)) ;
#6145 = CARTESIAN_POINT('Ctrl Pts',(30.8134076078136,58.766038570874,66.2356746117338)) ;
#6146 = CARTESIAN_POINT('Ctrl Pts',(30.7740741903988,58.5098890944364,66.0904525970946)) ;
#6147 = CARTESIAN_POINT('Ctrl Pts',(30.7303837591305,58.2537790654507,65.9462463126743)) ;
#6148 = CARTESIAN_POINT('Ctrl Pts',(30.6781206959667,57.9742522431174,65.7905703303672)) ;
#6149 = CARTESIAN_POINT('Ctrl Pts',(30.6736933470961,57.9507654759312,65.7775007825044)) ;
#6150 = CARTESIAN_POINT('Ctrl Pts',(30.6199239898024,57.6678169639212,65.6201853252031)) ;
#6151 = CARTESIAN_POINT('Ctrl Pts',(30.5662766775329,57.4086482068897,65.4774198047579)) ;
#6152 = CARTESIAN_POINT('Ctrl Pts',(30.5039911943873,57.1295421623675,65.3256766635461)) ;
#6153 = CARTESIAN_POINT('Ctrl Pts',(30.4995069859816,57.1095594972727,65.3148236099938)) ;
#6154 = CARTESIAN_POINT('Ctrl Pts',(30.4357484934212,56.8270031281969,65.1615169533963)) ;
#6155 = CARTESIAN_POINT('Ctrl Pts',(30.3722090617258,56.564476578324,65.0209656506715)) ;
#6156 = CARTESIAN_POINT('Ctrl Pts',(30.231391164111,56.0195645927232,64.733153409457)) ;
#6157 = CARTESIAN_POINT('Ctrl Pts',(30.1535492863315,55.7370242482923,64.5864375767227)) ;
#6158 = CARTESIAN_POINT('Ctrl Pts',(30.0671126637342,55.4412538423175,64.4356750041807)) ;
#6159 = CARTESIAN_POINT('Ctrl Pts',(30.0632845069496,55.4281899051451,64.4290213842513)) ;
#6160 = CARTESIAN_POINT('Ctrl Pts',(29.980209397746,55.1454478704628,64.2851365736848)) ;
#6161 = CARTESIAN_POINT('Ctrl Pts',(29.8965031969772,54.8754942178628,64.1500929953628)) ;
#6162 = CARTESIAN_POINT('Ctrl Pts',(29.8056563100459,54.5959998499613,64.013294987841)) ;
#6163 = CARTESIAN_POINT('Ctrl Pts',(29.8025330838997,54.5864072020384,64.0086033390302)) ;
#6164 = CARTESIAN_POINT('Ctrl Pts',(29.7102548621509,54.3034579214823,63.8703184606095)) ;
#6165 = CARTESIAN_POINT('Ctrl Pts',(29.6169368731029,54.0303635369496,63.7396467695494)) ;
#6166 = CARTESIAN_POINT('Ctrl Pts',(29.5174033116676,53.7513016854052,63.609207965875)) ;
#6167 = CARTESIAN_POINT('Ctrl Pts',(29.5152226671596,53.7451933157237,63.6063544218082)) ;
#6168 = CARTESIAN_POINT('Ctrl Pts',(29.4142735180212,53.4626708411959,63.4744482683264)) ;
#6169 = CARTESIAN_POINT('Ctrl Pts',(29.3114984136886,53.1862776071793,63.3487247516879)) ;
#6170 = CARTESIAN_POINT('Ctrl Pts',(29.2036980777988,52.9072592699432,63.2251533607292)) ;
#6171 = CARTESIAN_POINT('Ctrl Pts',(29.2026751441895,52.9046125716399,63.2239815002338)) ;
#6172 = CARTESIAN_POINT('Ctrl Pts',(29.2016518445348,52.9019658736982,63.2228099471636)) ;
#6173 = CARTESIAN_POINT('Ctrl Pts',(29.0937743039087,52.6229476375472,63.0993033444404)) ;
#6174 = CARTESIAN_POINT('Ctrl Pts',(28.9818294925969,52.3439334673732,62.9792145060285)) ;
#6175 = CARTESIAN_POINT('Ctrl Pts',(28.865782176196,52.0638397190087,62.8625418056171)) ;
#6176 = CARTESIAN_POINT('Ctrl Pts',(28.8654435444416,52.0630224673026,62.8622014135336)) ;
#6177 = CARTESIAN_POINT('Ctrl Pts',(28.8651048804777,52.0622052134034,62.8618610536397)) ;
#6178 = CARTESIAN_POINT('Ctrl Pts',(28.8065187928208,51.9208269928423,62.8029815840101)) ;
#6179 = CARTESIAN_POINT('Ctrl Pts',(28.7469483924193,51.7794019307221,62.7450428274934)) ;
#6180 = CARTESIAN_POINT('Ctrl Pts',(28.6276680578051,51.5007457293394,62.6327818911217)) ;
#6181 = CARTESIAN_POINT('Ctrl Pts',(28.5679909177056,51.3634912127544,62.5783831680472)) ;
#6182 = CARTESIAN_POINT('Ctrl Pts',(28.5056907825906,51.2220958064459,62.5233816695522)) ;
#6183 = CARTESIAN_POINT('Ctrl Pts',(28.5037978670285,51.2178014570208,62.5217121950908)) ;
#6184 = CARTESIAN_POINT('Ctrl Pts',(28.3806353677896,50.9385050159945,62.4131971637078)) ;
#6185 = CARTESIAN_POINT('Ctrl Pts',(28.2562425325705,50.6639128623093,62.3104626930187)) ;
#6186 = CARTESIAN_POINT('Ctrl Pts',(28.1251946565102,50.3820631700627,62.2090567779632)) ;
#6187 = CARTESIAN_POINT('Ctrl Pts',(28.1216204064942,50.374381438015,62.2062960797886)) ;
#6188 = CARTESIAN_POINT('Ctrl Pts',(27.9919781190897,50.0959566887312,62.1063464520381)) ;
#6189 = CARTESIAN_POINT('Ctrl Pts',(27.8630520121241,49.8255092945984,62.013263065848)) ;
#6190 = CARTESIAN_POINT('Ctrl Pts',(27.7261122130716,49.5442578124092,61.9207725737991)) ;
#6191 = CARTESIAN_POINT('Ctrl Pts',(27.7207631223362,49.533281035922,61.9171696510503)) ;
#6192 = CARTESIAN_POINT('Ctrl Pts',(27.5852110368569,49.2553528965713,61.8261180197291)) ;
#6193 = CARTESIAN_POINT('Ctrl Pts',(27.4522724975945,48.9886632517188,61.7426780639602)) ;
#6194 = CARTESIAN_POINT('Ctrl Pts',(27.3098129532935,48.7077521761841,61.6592875552603)) ;
#6195 = CARTESIAN_POINT('Ctrl Pts',(27.30260566038,48.6935533493115,61.6550846084527)) ;
#6196 = CARTESIAN_POINT('Ctrl Pts',(27.1527029138186,48.3985015698037,61.567999345586)) ;
#6197 = CARTESIAN_POINT('Ctrl Pts',(27.0073620617917,48.1176788676491,61.4897761421026)) ;
#6198 = CARTESIAN_POINT('Ctrl Pts',(26.7223664286535,47.5765229674271,61.3481705003658)) ;
#6199 = CARTESIAN_POINT('Ctrl Pts',(26.583304786595,47.3160356130356,61.2842340603531)) ;
#6200 = CARTESIAN_POINT('Ctrl Pts',(26.4311701471226,47.0348519182515,61.2197850173879)) ;
#6201 = CARTESIAN_POINT('Ctrl Pts',(26.4200560008957,47.0143316503714,61.2151078541788)) ;
#6202 = CARTESIAN_POINT('Ctrl Pts',(26.2692807870402,46.7362435810598,61.1520787578222)) ;
#6203 = CARTESIAN_POINT('Ctrl Pts',(26.1276801094453,46.4785159096922,61.0977909490593)) ;
#6204 = CARTESIAN_POINT('Ctrl Pts',(25.9713733923796,46.1967318999707,61.0431770974691)) ;
#6205 = CARTESIAN_POINT('Ctrl Pts',(25.9582359874009,46.1730689512029,61.038627292554)) ;
#6206 = CARTESIAN_POINT('Ctrl Pts',(25.8033345595273,45.8942981208808,60.9854572360907)) ;
#6207 = CARTESIAN_POINT('Ctrl Pts',(25.6599204237631,45.6388798207738,60.9409158281036)) ;
#6208 = CARTESIAN_POINT('Ctrl Pts',(25.5149631682039,45.3830586252743,60.9005821812565)) ;
#6209 = CARTESIAN_POINT('Origin',(23.47768801576,45.3830586252741,68.2224337400009)) ;
#6210 = CARTESIAN_POINT('',(17.4656830216285,45.3830634900533,63.5731543704541)) ;
#6211 = CARTESIAN_POINT('',(23.8549995017264,57.8256696110329,60.6318069295841)) ;
#6212 = CARTESIAN_POINT('Ctrl Pts',(17.4656832906589,45.3830652731062,63.5731539159243)) ;
#6213 = CARTESIAN_POINT('Ctrl Pts',(17.5413721503497,45.5935267840849,63.4752796473432)) ;
#6214 = CARTESIAN_POINT('Ctrl Pts',(17.6193703621342,45.8038922449965,63.3793583137785)) ;
#6215 = CARTESIAN_POINT('Ctrl Pts',(17.7183450921985,46.0632318316999,63.2635226696589)) ;
#6216 = CARTESIAN_POINT('Ctrl Pts',(17.737185181951,46.1122612415128,63.2417254911808)) ;
#6217 = CARTESIAN_POINT('Ctrl Pts',(17.841799005201,46.3827042839374,63.1220740583684)) ;
#6218 = CARTESIAN_POINT('Ctrl Pts',(17.9300056031499,46.6040125923438,63.0262673175482)) ;
#6219 = CARTESIAN_POINT('Ctrl Pts',(18.0360397662805,46.8632622432172,62.9168744495294)) ;
#6220 = CARTESIAN_POINT('Ctrl Pts',(18.0515947175824,46.9011261856486,62.9009670325896)) ;
#6221 = CARTESIAN_POINT('Ctrl Pts',(18.1632388279165,47.1717033808736,62.7877912727863)) ;
#6222 = CARTESIAN_POINT('Ctrl Pts',(18.2618711894541,47.4044689603724,62.6930575096971)) ;
#6223 = CARTESIAN_POINT('Ctrl Pts',(18.3747053074258,47.6638628918969,62.5903993209187)) ;
#6224 = CARTESIAN_POINT('Ctrl Pts',(18.3862969465815,47.6904386808303,62.5799183183686)) ;
#6225 = CARTESIAN_POINT('Ctrl Pts',(18.5047585919478,47.961299863605,62.4734695236722)) ;
#6226 = CARTESIAN_POINT('Ctrl Pts',(18.6142828302904,48.2057236046444,62.3805279202602)) ;
#6227 = CARTESIAN_POINT('Ctrl Pts',(18.733172538089,48.4649882125105,62.2852920020896)) ;
#6228 = CARTESIAN_POINT('Ctrl Pts',(18.740125235855,48.4801277704437,62.2797426177243)) ;
#6229 = CARTESIAN_POINT('Ctrl Pts',(18.8646014880951,48.7507815722807,62.1807478751498)) ;
#6230 = CARTESIAN_POINT('Ctrl Pts',(18.984910206447,49.006060387104,62.0907576267275)) ;
#6231 = CARTESIAN_POINT('Ctrl Pts',(19.1094339115856,49.2650911286613,62.0032407968347)) ;
#6232 = CARTESIAN_POINT('Ctrl Pts',(19.111223731813,49.2688131587655,62.001984041469)) ;
#6233 = CARTESIAN_POINT('Ctrl Pts',(19.1130140805669,49.2725351845606,62.0007280675306)) ;
#6234 = CARTESIAN_POINT('Ctrl Pts',(19.2376113588956,49.5315653220715,61.9133199946472)) ;
#6235 = CARTESIAN_POINT('Ctrl Pts',(19.3647683149683,49.7905771610406,61.8296961034925)) ;
#6236 = CARTESIAN_POINT('Ctrl Pts',(19.4983327806004,50.0572510953383,61.747501126198)) ;
#6237 = CARTESIAN_POINT('Ctrl Pts',(19.5021804841665,50.0649289262843,61.7451379880606)) ;
#6238 = CARTESIAN_POINT('Ctrl Pts',(19.6320501700217,50.3239244418398,61.6655353117229)) ;
#6239 = CARTESIAN_POINT('Ctrl Pts',(19.7602296512367,50.5754015948895,61.5920211044488)) ;
#6240 = CARTESIAN_POINT('Ctrl Pts',(19.9004727840933,50.8461423400857,61.5169391572625)) ;
#6241 = CARTESIAN_POINT('Ctrl Pts',(19.9103830129235,50.8652509230937,61.5116617200819)) ;
#6242 = CARTESIAN_POINT('Ctrl Pts',(20.0450514572642,51.1245997230103,61.4403298060522)) ;
#6243 = CARTESIAN_POINT('Ctrl Pts',(20.1718845771644,51.3650618940538,61.3776143442512)) ;
#6244 = CARTESIAN_POINT('Ctrl Pts',(20.3164323919744,51.6358437425513,61.3110820716862)) ;
#6245 = CARTESIAN_POINT('Ctrl Pts',(20.332759976084,51.6663832990502,61.3036369158996)) ;
#6246 = CARTESIAN_POINT('Ctrl Pts',(20.4940604089653,51.9676379850866,61.2307770046641)) ;
#6247 = CARTESIAN_POINT('Ctrl Pts',(20.6409772855714,52.2381644565101,61.1698912576762)) ;
#6248 = CARTESIAN_POINT('Ctrl Pts',(20.9091109436541,52.7256472364568,61.0685042200231)) ;
#6249 = CARTESIAN_POINT('Ctrl Pts',(21.0295354376883,52.9427458528919,61.0264045298722)) ;
#6250 = CARTESIAN_POINT('Ctrl Pts',(21.1807822532647,53.2131562545791,60.9777662096284)) ;
#6251 = CARTESIAN_POINT('Ctrl Pts',(21.2106594814961,53.2664641483671,60.9683615759732)) ;
#6252 = CARTESIAN_POINT('Ctrl Pts',(21.3561278084265,53.5254861983863,60.9235574150852)) ;
#6253 = CARTESIAN_POINT('Ctrl Pts',(21.472593077294,53.7311956119202,60.8907073760518)) ;
#6254 = CARTESIAN_POINT('Ctrl Pts',(21.6266498253265,54.0017837515366,60.8511989830966)) ;
#6255 = CARTESIAN_POINT('Ctrl Pts',(21.6635854730858,54.0665473332689,60.842021815219)) ;
#6256 = CARTESIAN_POINT('Ctrl Pts',(21.8116789708385,54.3258257235488,60.8064058684495)) ;
#6257 = CARTESIAN_POINT('Ctrl Pts',(21.923502442178,54.5205088505476,60.7821673262479)) ;
#6258 = CARTESIAN_POINT('Ctrl Pts',(22.0798761893219,54.7914199725089,60.7519504321609)) ;
#6259 = CARTESIAN_POINT('Ctrl Pts',(22.1239665319832,54.8676682916975,60.7438344836362)) ;
#6260 = CARTESIAN_POINT('Ctrl Pts',(22.3249401696415,55.2146576988347,60.708678399366)) ;
#6261 = CARTESIAN_POINT('Ctrl Pts',(22.4823402930707,55.4852678000144,60.6862178575749)) ;
#6262 = CARTESIAN_POINT('Ctrl Pts',(22.7405323613007,55.9272948494774,60.6575962799744)) ;
#6263 = CARTESIAN_POINT('Ctrl Pts',(22.8409757562831,56.0987899530342,60.6484819599386)) ;
#6264 = CARTESIAN_POINT('Ctrl Pts',(22.9995283082329,56.3691923043824,60.637268359989)) ;
#6265 = CARTESIAN_POINT('Ctrl Pts',(23.0575505347489,56.4680781862304,60.6338330179249)) ;
#6266 = CARTESIAN_POINT('Ctrl Pts',(23.3616336382064,56.9862401445896,60.6193287252703)) ;
#6267 = CARTESIAN_POINT('Ctrl Pts',(23.6084290417824,57.4056326748909,60.6195531644626)) ;
#6268 = CARTESIAN_POINT('Ctrl Pts',(23.8549866701408,57.8256477522086,60.6318062918727)) ;
#6269 = CARTESIAN_POINT('',(23.8550298361323,57.8271591833517,60.6318070761082)) ;
#6270 = CARTESIAN_POINT('Ctrl Pts',(23.8550132718507,57.825693068674,60.6318076139396)) ;
#6271 = CARTESIAN_POINT('Ctrl Pts',(23.8550297465186,57.8261751444418,60.6318084307449)) ;
#6272 = CARTESIAN_POINT('Ctrl Pts',(23.8550297816016,57.8266671622709,60.6318080026266)) ;
#6273 = CARTESIAN_POINT('Ctrl Pts',(23.8550298361323,57.8271591833517,60.6318070761082)) ;
#6274 = CARTESIAN_POINT('',(23.8550298272675,58.7660385728413,60.6318072809575)) ;
#6275 = CARTESIAN_POINT('',(23.8550298361323,43.8830586252741,60.6318070761082)) ;
#6276 = CARTESIAN_POINT('',(17.1437460318932,45.3830586252742,64.0222933742113)) ;
#6277 = CARTESIAN_POINT('Ctrl Pts',(23.8550298204266,58.7660385708796,60.6318074859001)) ;
#6278 = CARTESIAN_POINT('Ctrl Pts',(23.7047607826612,58.5098890944426,60.624339718359)) ;
#6279 = CARTESIAN_POINT('Ctrl Pts',(23.5541113704526,58.2537790654492,60.6213295951355)) ;
#6280 = CARTESIAN_POINT('Ctrl Pts',(23.3899045383306,57.9742522431133,60.6229281977702)) ;
#6281 = CARTESIAN_POINT('Ctrl Pts',(23.3761065336288,57.9507654759275,60.6231001443651)) ;
#6282 = CARTESIAN_POINT('Ctrl Pts',(23.2098749976631,57.6678169639206,60.6256246922118)) ;
#6283 = CARTESIAN_POINT('Ctrl Pts',(23.0575189879674,57.4086482068946,60.6325293460982)) ;
#6284 = CARTESIAN_POINT('Ctrl Pts',(22.8939554119029,57.1295421623652,60.6448751513013)) ;
#6285 = CARTESIAN_POINT('Ctrl Pts',(22.8822478479962,57.1095594972706,60.6457861089375)) ;
#6286 = CARTESIAN_POINT('Ctrl Pts',(22.7167420955076,56.8270031281923,60.6590496765166)) ;
#6287 = CARTESIAN_POINT('Ctrl Pts',(22.5634350990063,56.5644765783291,60.6760465259443)) ;
#6288 = CARTESIAN_POINT('Ctrl Pts',(22.2461942679969,56.0195645927191,60.7210334313653)) ;
#6289 = CARTESIAN_POINT('Ctrl Pts',(22.0826047561317,55.7370242483032,60.7497277708092)) ;
#6290 = CARTESIAN_POINT('Ctrl Pts',(21.9125106437908,55.4412538423216,60.7853456869443)) ;
#6291 = CARTESIAN_POINT('Ctrl Pts',(21.9049997096968,55.428189905149,60.7869303987674)) ;
#6292 = CARTESIAN_POINT('Ctrl Pts',(21.7424855024646,55.1454478704628,60.8214766710187)) ;
#6293 = CARTESIAN_POINT('Ctrl Pts',(21.5881847887512,54.8754942178679,60.8593552380298)) ;
#6294 = CARTESIAN_POINT('Ctrl Pts',(21.430008920329,54.5959998499605,60.9034828527113)) ;
#6295 = CARTESIAN_POINT('Ctrl Pts',(21.4245817671989,54.5864072020377,60.9050034180752)) ;
#6296 = CARTESIAN_POINT('Ctrl Pts',(21.2645494937397,54.3034579214823,60.9500328446847)) ;
#6297 = CARTESIAN_POINT('Ctrl Pts',(21.111436485969,54.0303635369511,60.9984037530338)) ;
#6298 = CARTESIAN_POINT('Ctrl Pts',(20.9566242497591,53.7513016854048,61.0527579881668)) ;
#6299 = CARTESIAN_POINT('Ctrl Pts',(20.9532365118681,53.7451933157233,61.053950110725)) ;
#6300 = CARTESIAN_POINT('Ctrl Pts',(20.7965913024079,53.4626708411959,61.1091972137392)) ;
#6301 = CARTESIAN_POINT('Ctrl Pts',(20.6452618788204,53.186277607177,61.1680914431933)) ;
#6302 = CARTESIAN_POINT('Ctrl Pts',(20.4944263664219,52.9072592699496,61.2324299952799)) ;
#6303 = CARTESIAN_POINT('Ctrl Pts',(20.4929957569922,52.9046125716463,61.2330407381467)) ;
#6304 = CARTESIAN_POINT('Ctrl Pts',(20.3407675741267,52.6229476375602,61.2980839229628)) ;
#6305 = CARTESIAN_POINT('Ctrl Pts',(20.1919634527057,52.3439334673782,61.3674402733172)) ;
#6306 = CARTESIAN_POINT('Ctrl Pts',(20.0451405277899,52.0638397190112,61.4417539825704)) ;
#6307 = CARTESIAN_POINT('Ctrl Pts',(20.0447121527138,52.0630224673051,61.4419708535685)) ;
#6308 = CARTESIAN_POINT('Ctrl Pts',(20.0442837982987,52.0622052134059,61.4421877651467)) ;
#6309 = CARTESIAN_POINT('Ctrl Pts',(19.9701819983144,51.9208269928453,61.4797116888403)) ;
#6310 = CARTESIAN_POINT('Ctrl Pts',(19.8966707002981,51.7794019307423,61.5184624459233)) ;
#6311 = CARTESIAN_POINT('Ctrl Pts',(19.7530445547343,51.5007457293231,61.5972142482874)) ;
#6312 = CARTESIAN_POINT('Ctrl Pts',(19.6828670441985,51.3634912127728,61.6371604513572)) ;
#6313 = CARTESIAN_POINT('Ctrl Pts',(19.6113057101537,51.2220958064568,61.6794150030693)) ;
#6314 = CARTESIAN_POINT('Ctrl Pts',(19.6091330025111,51.2178014570316,61.680699376769)) ;
#6315 = CARTESIAN_POINT('Ctrl Pts',(19.4678697694841,50.9385050159871,61.7643008853794)) ;
#6316 = CARTESIAN_POINT('Ctrl Pts',(19.3317239816368,50.6639128622978,61.8508588045359)) ;
#6317 = CARTESIAN_POINT('Ctrl Pts',(19.1947852045447,50.3820631700569,61.9441565899327)) ;
#6318 = CARTESIAN_POINT('Ctrl Pts',(19.1910551205589,50.3743814380095,61.9467028010492)) ;
#6319 = CARTESIAN_POINT('Ctrl Pts',(19.0559357057821,50.0959566887385,62.03911380972)) ;
#6320 = CARTESIAN_POINT('Ctrl Pts',(18.9275677867106,49.8255092946014,62.132965475648)) ;
#6321 = CARTESIAN_POINT('Ctrl Pts',(18.7972873764406,49.5442578124104,62.2346218300143)) ;
#6322 = CARTESIAN_POINT('Ctrl Pts',(18.792207833341,49.5332810359232,62.2385957532556)) ;
#6323 = CARTESIAN_POINT('Ctrl Pts',(18.663724688025,49.2553528965829,62.3393769459986)) ;
#6324 = CARTESIAN_POINT('Ctrl Pts',(18.5432883065279,48.9886632517177,62.4400246456917)) ;
#6325 = CARTESIAN_POINT('Ctrl Pts',(18.4199567996313,48.7077521761834,62.5497426392499)) ;
#6326 = CARTESIAN_POINT('Ctrl Pts',(18.4137323836886,48.6935533493109,62.5552984001501)) ;
#6327 = CARTESIAN_POINT('Ctrl Pts',(18.284586880776,48.3985015698064,62.6709535578915)) ;
#6328 = CARTESIAN_POINT('Ctrl Pts',(18.1652794001422,48.1176788676501,62.7850086230464)) ;
#6329 = CARTESIAN_POINT('Ctrl Pts',(17.9425359378238,47.5765229674263,63.012297027301)) ;
#6330 = CARTESIAN_POINT('Ctrl Pts',(17.8387563592619,47.3160356130502,63.1247950616225)) ;
#6331 = CARTESIAN_POINT('Ctrl Pts',(17.7304494879593,47.0348519182585,63.2495678522903)) ;
#6332 = CARTESIAN_POINT('Ctrl Pts',(17.7225667813501,47.0143316503778,63.2586927105645)) ;
#6333 = CARTESIAN_POINT('Ctrl Pts',(17.6160304451424,46.7362435810516,63.3826113982718)) ;
#6334 = CARTESIAN_POINT('Ctrl Pts',(17.5206426550712,46.478515909689,63.5005057899146)) ;
#6335 = CARTESIAN_POINT('Ctrl Pts',(17.4204003637262,46.1967318999692,63.6322857034532)) ;
#6336 = CARTESIAN_POINT('Ctrl Pts',(17.4120135607131,46.1730689512017,63.6433741510259)) ;
#6337 = CARTESIAN_POINT('Ctrl Pts',(17.3135786583707,45.8942981208826,63.7742637123565)) ;
#6338 = CARTESIAN_POINT('Ctrl Pts',(17.2268998568785,45.6388798207739,63.8968946086769)) ;
#6339 = CARTESIAN_POINT('Ctrl Pts',(17.1437460237932,45.3830586252743,64.0222933688401)) ;
#6340 = CARTESIAN_POINT('Origin',(23.47768801576,45.3830586252741,68.2224337400009)) ;
#6341 = CARTESIAN_POINT('',(25.608724379063,45.3830634900508,75.5175476338228)) ;
#6342 = CARTESIAN_POINT('',(18.7107781165901,57.8256696109658,74.1416017005878)) ;
#6343 = CARTESIAN_POINT('Ctrl Pts',(25.6087238942477,45.3830652731009,75.5175478434128)) ;
#6344 = CARTESIAN_POINT('Ctrl Pts',(25.4899612688168,45.5935267840753,75.5522409945192)) ;
#6345 = CARTESIAN_POINT('Ctrl Pts',(25.3704782447056,45.8038922449995,75.5839967849029)) ;
#6346 = CARTESIAN_POINT('Ctrl Pts',(25.2223195227794,46.0632318317002,75.6195339028655)) ;
#6347 = CARTESIAN_POINT('Ctrl Pts',(25.1942655099435,46.1122612415132,75.6260942637752)) ;
#6348 = CARTESIAN_POINT('Ctrl Pts',(25.0393018014623,46.3827042839383,75.6614038438299)) ;
#6349 = CARTESIAN_POINT('Ctrl Pts',(24.9116273753729,46.6040125923255,75.6870665879016)) ;
#6350 = CARTESIAN_POINT('Ctrl Pts',(24.7615444208957,46.8632622432174,75.7132419598636)) ;
#6351 = CARTESIAN_POINT('Ctrl Pts',(24.7396100558675,46.9011261856493,75.716968359529)) ;
#6352 = CARTESIAN_POINT('Ctrl Pts',(24.5827650307564,47.1717033808735,75.7429067110011)) ;
#6353 = CARTESIAN_POINT('Ctrl Pts',(24.4472866652317,47.4044689603717,75.7615732877718)) ;
#6354 = CARTESIAN_POINT('Ctrl Pts',(24.2956609768662,47.6638628918981,75.778303276605)) ;
#6355 = CARTESIAN_POINT('Ctrl Pts',(24.2801225650689,47.690438680832,75.7799691912404)) ;
#6356 = CARTESIAN_POINT('Ctrl Pts',(24.1217160491427,47.9612998636085,75.7964580670714)) ;
#6357 = CARTESIAN_POINT('Ctrl Pts',(23.9784793752071,48.2057236046616,75.8072726716508)) ;
#6358 = CARTESIAN_POINT('Ctrl Pts',(23.8263173129591,48.4649882125116,75.814438531032)) ;
#6359 = CARTESIAN_POINT('Ctrl Pts',(23.8174306160203,48.4801277704447,75.8148413840814)) ;
#6360 = CARTESIAN_POINT('Ctrl Pts',(23.6585395628197,48.7507815722807,75.8217645078505)) ;
#6361 = CARTESIAN_POINT('Ctrl Pts',(23.5083128242133,49.0060603870971,75.8238524577829)) ;
#6362 = CARTESIAN_POINT('Ctrl Pts',(23.3561299286236,49.265091128657,75.8214618630187)) ;
#6363 = CARTESIAN_POINT('Ctrl Pts',(23.3539432313732,49.2688131587613,75.8214265695334)) ;
#6364 = CARTESIAN_POINT('Ctrl Pts',(23.1995780740611,49.5315653220715,75.8188685069308)) ;
#6365 = CARTESIAN_POINT('Ctrl Pts',(23.0475530456853,49.7905771610406,75.811780672505)) ;
#6366 = CARTESIAN_POINT('Ctrl Pts',(22.8911841276718,50.0572510953345,75.7997705828591)) ;
#6367 = CARTESIAN_POINT('Ctrl Pts',(22.8866822523511,50.0649289262804,75.799420778361)) ;
#6368 = CARTESIAN_POINT('Ctrl Pts',(22.7348261902374,50.3239244418333,75.7874852102496)) ;
#6369 = CARTESIAN_POINT('Ctrl Pts',(22.5879162447379,50.5754015948824,75.7716174445575)) ;
#6370 = CARTESIAN_POINT('Ctrl Pts',(22.4303251056493,50.8461423400821,75.7499271705742)) ;
#6371 = CARTESIAN_POINT('Ctrl Pts',(22.4192055623634,50.8652509230905,75.7483716205869)) ;
#6372 = CARTESIAN_POINT('Ctrl Pts',(22.2683286552059,51.1245997230184,75.7269242257462)) ;
#6373 = CARTESIAN_POINT('Ctrl Pts',(22.1288552822128,51.3650618940492,75.7031114627724)) ;
#6374 = CARTESIAN_POINT('Ctrl Pts',(21.9728069549191,51.6358437425482,75.6719741281559)) ;
#6375 = CARTESIAN_POINT('Ctrl Pts',(21.9552215091257,51.6663832990475,75.668400272568)) ;
#6376 = CARTESIAN_POINT('Ctrl Pts',(21.7819007364219,51.9676379851017,75.6325351633311)) ;
#6377 = CARTESIAN_POINT('Ctrl Pts',(21.6272547423225,52.2381644564706,75.5954371939749)) ;
#6378 = CARTESIAN_POINT('Ctrl Pts',(21.3507362506827,52.7256472364779,75.5198560205866)) ;
#6379 = CARTESIAN_POINT('Ctrl Pts',(21.2285652114554,52.9427458528933,75.4831316437627)) ;
#6380 = CARTESIAN_POINT('Ctrl Pts',(21.077615079979,53.2131562545778,75.4335802237679)) ;
#6381 = CARTESIAN_POINT('Ctrl Pts',(21.0479159896309,53.266464148367,75.4236273380877)) ;
#6382 = CARTESIAN_POINT('Ctrl Pts',(20.9038944160104,53.5254861983966,75.3743705284267)) ;
#6383 = CARTESIAN_POINT('Ctrl Pts',(20.7903632657492,53.7311956119258,75.332490200822)) ;
#6384 = CARTESIAN_POINT('Ctrl Pts',(20.6425062877679,54.0017837515375,75.2739008776323)) ;
#6385 = CARTESIAN_POINT('Ctrl Pts',(20.6072305170954,54.0665473332692,75.2596151333686)) ;
#6386 = CARTESIAN_POINT('Ctrl Pts',(20.4664858323946,54.3258257235614,75.2013818656345)) ;
#6387 = CARTESIAN_POINT('Ctrl Pts',(20.3617716860696,54.5205088505461,75.1552630708817)) ;
#6388 = CARTESIAN_POINT('Ctrl Pts',(20.2175016224408,54.7914199725073,75.0877948692979)) ;
#6389 = CARTESIAN_POINT('Ctrl Pts',(20.1770613510901,54.8676682916958,75.0684451563956)) ;
#6390 = CARTESIAN_POINT('Ctrl Pts',(19.9938060349454,55.2146576988565,74.9787576857131)) ;
#6391 = CARTESIAN_POINT('Ctrl Pts',(19.8532646849623,55.4852677999964,74.904411174471)) ;
#6392 = CARTESIAN_POINT('Ctrl Pts',(19.6275595727133,55.9272948494813,74.7758050271755)) ;
#6393 = CARTESIAN_POINT('Ctrl Pts',(19.5409418963078,56.0987899530378,74.724139520722)) ;
#6394 = CARTESIAN_POINT('Ctrl Pts',(19.4060789986044,56.3691923043834,74.6400166619002)) ;
#6395 = CARTESIAN_POINT('Ctrl Pts',(19.3571187878985,56.4680781862293,74.6086913029594)) ;
#6396 = CARTESIAN_POINT('Ctrl Pts',(19.1025849801468,56.9862401445611,74.4416899585013)) ;
#6397 = CARTESIAN_POINT('Ctrl Pts',(18.9030552265289,57.405632674834,74.2964456847875)) ;
#6398 = CARTESIAN_POINT('Ctrl Pts',(18.710788122709,57.8256477521734,74.1416097587122)) ;
#6399 = CARTESIAN_POINT('',(18.7107539506873,57.8265499698715,74.1415834028921)) ;
#6400 = CARTESIAN_POINT('Ctrl Pts',(18.7107673785944,57.8256930685744,74.1415930530686)) ;
#6401 = CARTESIAN_POINT('Ctrl Pts',(18.7107545283917,57.8259720707006,74.1415827059215)) ;
#6402 = CARTESIAN_POINT('Ctrl Pts',(18.7107544336864,57.8262610185798,74.1415828059768)) ;
#6403 = CARTESIAN_POINT('Ctrl Pts',(18.7107542314619,57.8265499693315,74.1415830471385)) ;
#6404 = CARTESIAN_POINT('',(18.7107537892754,58.7660385728357,74.1415835914416)) ;
#6405 = CARTESIAN_POINT('',(18.7107536616963,43.8830586252741,74.1415837519576)) ;
#6406 = CARTESIAN_POINT('',(26.1331741575238,45.3830586252742,75.3434163616778)) ;
#6407 = CARTESIAN_POINT('Ctrl Pts',(18.7107539152721,58.766038570874,74.1415834296607)) ;
#6408 = CARTESIAN_POINT('Ctrl Pts',(18.827934676918,58.5098890944341,74.2359509047808)) ;
#6409 = CARTESIAN_POINT('Ctrl Pts',(18.948043305545,58.2537790654364,74.3269356483841)) ;
#6410 = CARTESIAN_POINT('Ctrl Pts',(19.0818290583823,57.9742522431095,74.4221607059362)) ;
#6411 = CARTESIAN_POINT('Ctrl Pts',(19.0930929463476,57.9507654759241,74.430131861894)) ;
#6412 = CARTESIAN_POINT('Ctrl Pts',(19.2290609759425,57.66781696392,74.5257979050929)) ;
#6413 = CARTESIAN_POINT('Ctrl Pts',(19.3563780307201,57.4086482069147,74.6097645383633)) ;
#6414 = CARTESIAN_POINT('Ctrl Pts',(19.49596042564,57.1295421623709,74.6959168299655)) ;
#6415 = CARTESIAN_POINT('Ctrl Pts',(19.5059674912669,57.1095594972761,74.7020613831611)) ;
#6416 = CARTESIAN_POINT('Ctrl Pts',(19.6476605871094,56.8270031281938,74.7886127720636)) ;
#6417 = CARTESIAN_POINT('Ctrl Pts',(19.7816790500644,56.5644765783529,74.8649736236426)) ;
#6418 = CARTESIAN_POINT('Ctrl Pts',(20.0647749132364,56.0195645927199,75.0150479345363)) ;
#6419 = CARTESIAN_POINT('Ctrl Pts',(20.2139877179671,55.7370242483082,75.0879892287777)) ;
#6420 = CARTESIAN_POINT('Ctrl Pts',(20.3725324313107,55.4412538423241,75.1591525400536)) ;
#6421 = CARTESIAN_POINT('Ctrl Pts',(20.379540374875,55.4281899051513,75.1622852975488)) ;
#6422 = CARTESIAN_POINT('Ctrl Pts',(20.5313229197007,55.1454478704631,75.2298602305026)) ;
#6423 = CARTESIAN_POINT('Ctrl Pts',(20.6784192824002,54.8754942178506,75.2899115100048)) ;
#6424 = CARTESIAN_POINT('Ctrl Pts',(20.8323238091829,54.5959998499574,75.3471849625336)) ;
#6425 = CARTESIAN_POINT('Ctrl Pts',(20.8376082341926,54.5864072020347,75.349144799885)) ;
#6426 = CARTESIAN_POINT('Ctrl Pts',(20.9935446959547,54.3034579214823,75.4067798387431)) ;
#6427 = CARTESIAN_POINT('Ctrl Pts',(21.1458474278724,54.0303635369504,75.4576445197581)) ;
#6428 = CARTESIAN_POINT('Ctrl Pts',(21.3030417757119,53.7513016854057,75.5046673691372)) ;
#6429 = CARTESIAN_POINT('Ctrl Pts',(21.3064832252968,53.7451933157242,75.5056941840992)) ;
#6430 = CARTESIAN_POINT('Ctrl Pts',(21.4656852942199,53.4626708411959,75.5530720828333)) ;
#6431 = CARTESIAN_POINT('Ctrl Pts',(21.6227305291694,53.1862776071773,75.5943748537571)) ;
#6432 = CARTESIAN_POINT('Ctrl Pts',(21.7825762741261,52.9072592699501,75.6309827614355)) ;
#6433 = CARTESIAN_POINT('Ctrl Pts',(21.7840926471172,52.9046125716468,75.6313295512016)) ;
#6434 = CARTESIAN_POINT('Ctrl Pts',(21.945479258876,52.6229476375612,75.6681859901889)) ;
#6435 = CARTESIAN_POINT('Ctrl Pts',(22.1066309618375,52.3439334673839,75.6995403921371)) ;
#6436 = CARTESIAN_POINT('Ctrl Pts',(22.2690937055957,52.063839719014,75.7257196883994)) ;
#6437 = CARTESIAN_POINT('Ctrl Pts',(22.2695677418866,52.0630224673079,75.7257960286286)) ;
#6438 = CARTESIAN_POINT('Ctrl Pts',(22.2700417853147,52.0622052134087,75.7258723238834)) ;
#6439 = CARTESIAN_POINT('Ctrl Pts',(22.3520474097712,51.9208269928421,75.7390707771187)) ;
#6440 = CARTESIAN_POINT('Ctrl Pts',(22.4342964226827,51.7794019307305,75.7509296129456)) ;
#6441 = CARTESIAN_POINT('Ctrl Pts',(22.5967815632748,51.5007457293469,75.771639396698)) ;
#6442 = CARTESIAN_POINT('Ctrl Pts',(22.6770361509753,51.3634912127619,75.78057154529)) ;
#6443 = CARTESIAN_POINT('Ctrl Pts',(22.7597670886974,51.2220958064525,75.7884495916514)) ;
#6444 = CARTESIAN_POINT('Ctrl Pts',(22.7622797820233,51.2178014570273,75.7886875970111)) ;
#6445 = CARTESIAN_POINT('Ctrl Pts',(22.9257038720592,50.9385050159947,75.8040850008551)) ;
#6446 = CARTESIAN_POINT('Ctrl Pts',(23.086725596493,50.6639128622994,75.8140826595182)) ;
#6447 = CARTESIAN_POINT('Ctrl Pts',(23.2523504566757,50.3820631700578,75.8190937592362)) ;
#6448 = CARTESIAN_POINT('Ctrl Pts',(23.2568647833541,50.3743814380103,75.8192263195284)) ;
#6449 = CARTESIAN_POINT('Ctrl Pts',(23.4204965142258,50.0959566887354,75.8238854423506)) ;
#6450 = CARTESIAN_POINT('Ctrl Pts',(23.5795129674232,49.8255092946031,75.8234106193621)) ;
#6451 = CARTESIAN_POINT('Ctrl Pts',(23.7446641392626,49.5442578124114,75.8177458049129)) ;
#6452 = CARTESIAN_POINT('Ctrl Pts',(23.7511093894287,49.5332810359241,75.8175165139986)) ;
#6453 = CARTESIAN_POINT('Ctrl Pts',(23.9142921362852,49.2553528965747,75.811503314341)) ;
#6454 = CARTESIAN_POINT('Ctrl Pts',(24.0708864491977,48.98866325171,75.8008683437293)) ;
#6455 = CARTESIAN_POINT('Ctrl Pts',(24.2351543527481,48.7077521761783,75.7845970632484)) ;
#6456 = CARTESIAN_POINT('Ctrl Pts',(24.2434556053485,48.693553349306,75.7837609781587)) ;
#6457 = CARTESIAN_POINT('Ctrl Pts',(24.4159169080327,48.3985015698049,75.76610381207)) ;
#6458 = CARTESIAN_POINT('Ctrl Pts',(24.5794785726484,48.1176788676782,75.7439585036729)) ;
#6459 = CARTESIAN_POINT('Ctrl Pts',(24.893278591109,47.5765229673886,75.6910036441987)) ;
#6460 = CARTESIAN_POINT('Ctrl Pts',(25.0433627192943,47.3160356130354,75.6609909283725)) ;
#6461 = CARTESIAN_POINT('Ctrl Pts',(25.2043244250407,47.0348519182514,75.6237088019572)) ;
#6462 = CARTESIAN_POINT('Ctrl Pts',(25.2160651257732,47.0143316503714,75.6209599752349)) ;
#6463 = CARTESIAN_POINT('Ctrl Pts',(25.3750924094244,46.7362435810525,75.5833281382101)) ;
#6464 = CARTESIAN_POINT('Ctrl Pts',(25.5215593373602,46.4785159096822,75.5440171080885)) ;
#6465 = CARTESIAN_POINT('Ctrl Pts',(25.6801153443456,46.196731899966,75.4963258590251)) ;
#6466 = CARTESIAN_POINT('Ctrl Pts',(25.6934180364662,46.1730689511987,75.4922847556223)) ;
#6467 = CARTESIAN_POINT('Ctrl Pts',(25.8499884991378,45.894298120883,75.444251460025)) ;
#6468 = CARTESIAN_POINT('Ctrl Pts',(25.9921937549264,45.638879820774,75.3959895020703)) ;
#6469 = CARTESIAN_POINT('Ctrl Pts',(26.1331741609196,45.3830586252743,75.3434163707842)) ;
#6470 = CARTESIAN_POINT('Origin',(23.47768801576,45.3830586252741,68.2224337400009)) ;
#6471 = CARTESIAN_POINT('Origin',(58.47768801576,45.3830586252741,68.1724337400008)) ;
#6472 = CARTESIAN_POINT('',(31.2758081909614,45.3830610445957,68.222429730099)) ;
#6473 = CARTESIAN_POINT('',(51.7933248065259,45.3830586252741,68.2224337400008)) ;
#6474 = CARTESIAN_POINT('',(31.2758081909603,45.3830586252741,68.2224337400009)) ;
#6475 = CARTESIAN_POINT('Ctrl Pts',(31.2758081909618,45.3830586252741,68.2224282704332)) ;
#6476 = CARTESIAN_POINT('Ctrl Pts',(31.2619815052159,45.3830586252741,68.2224282693451)) ;
#6477 = CARTESIAN_POINT('Ctrl Pts',(31.248244467626,45.3830586252741,68.2241023785107)) ;
#6478 = CARTESIAN_POINT('Ctrl Pts',(31.2203040134215,45.3830586252741,68.23092080966)) ;
#6479 = CARTESIAN_POINT('Ctrl Pts',(31.2063378307747,45.3830586252741,68.2362851030096)) ;
#6480 = CARTESIAN_POINT('Ctrl Pts',(31.1691061004754,45.3830586252741,68.2559255255466)) ;
#6481 = CARTESIAN_POINT('Ctrl Pts',(31.1481050711888,45.3830586252741,68.2736067598549)) ;
#6482 = CARTESIAN_POINT('Ctrl Pts',(31.1120389980945,45.3830586252741,68.3173139549359)) ;
#6483 = CARTESIAN_POINT('Ctrl Pts',(31.097829072345,45.3830586252736,68.3436048263349)) ;
#6484 = CARTESIAN_POINT('Ctrl Pts',(31.0797781562955,45.3830586252736,68.3967923257375)) ;
#6485 = CARTESIAN_POINT('Ctrl Pts',(31.0750788916455,45.3830586252741,68.4233474108136)) ;
#6486 = CARTESIAN_POINT('Ctrl Pts',(31.0742802400156,45.3830586252741,68.4500085087909)) ;
#6487 = CARTESIAN_POINT('',(31.2729697953901,45.3830674541112,68.1224191093439)) ;
#6488 = CARTESIAN_POINT('Ctrl Pts',(31.0707352963726,45.3830586252741,67.897420987276)) ;
#6489 = CARTESIAN_POINT('Ctrl Pts',(31.0718578683993,45.3830586252741,67.9236365013638)) ;
#6490 = CARTESIAN_POINT('Ctrl Pts',(31.0767528122927,45.3830586252745,67.9497000931763)) ;
#6491 = CARTESIAN_POINT('Ctrl Pts',(31.0950990117691,45.3830586252745,68.0023971425259)) ;
#6492 = CARTESIAN_POINT('Ctrl Pts',(31.1095495115892,45.3830586252741,68.0286334382962)) ;
#6493 = CARTESIAN_POINT('Ctrl Pts',(31.1460384959778,45.3830586252741,68.0721480965577)) ;
#6494 = CARTESIAN_POINT('Ctrl Pts',(31.1672243458983,45.3830586252741,68.0897024121122)) ;
#6495 = CARTESIAN_POINT('Ctrl Pts',(31.2044592007308,45.3830586252741,68.1089700371596)) ;
#6496 = CARTESIAN_POINT('Ctrl Pts',(31.2182435715767,45.3830586252741,68.1141717381528)) ;
#6497 = CARTESIAN_POINT('Ctrl Pts',(31.2457964764012,45.3830586252741,68.1207877758046)) ;
#6498 = CARTESIAN_POINT('Ctrl Pts',(31.2593403999271,45.3830586252741,68.1224138614655)) ;
#6499 = CARTESIAN_POINT('Ctrl Pts',(31.2729697270889,45.3830586252741,68.1224137848817)) ;
#6500 = CARTESIAN_POINT('',(50.6143421942707,45.3830586252741,68.1224337400008)) ;
#6501 = CARTESIAN_POINT('',(50.6143421942707,45.3830586252741,68.1224337400008)) ;
#6502 = CARTESIAN_POINT('Origin',(50.6143421942707,45.3830586252741,75.1224337400008)) ;
#6503 = CARTESIAN_POINT('Ctrl Pts',(30.9776880157584,45.3830502402145,68.2224288733178)) ;
#6504 = CARTESIAN_POINT('Ctrl Pts',(30.9776882407603,45.980480894371,68.5691772383443)) ;
#6505 = CARTESIAN_POINT('Ctrl Pts',(30.9456943379727,46.5779115664506,68.9144464359756)) ;
#6506 = CARTESIAN_POINT('Ctrl Pts',(30.9137006601855,47.1753380370388,69.2597132054666)) ;
#6507 = CARTESIAN_POINT('Ctrl Pts',(30.8499862633892,47.772764507627,69.6005551236251)) ;
#6508 = CARTESIAN_POINT('Ctrl Pts',(30.786271866593,48.3701909782152,69.9413970417837)) ;
#6509 = CARTESIAN_POINT('Ctrl Pts',(30.6913803395561,48.9676174488035,70.2749061655415)) ;
#6510 = CARTESIAN_POINT('Ctrl Pts',(30.5964888125192,49.5650439193917,70.6084152892993)) ;
#6511 = CARTESIAN_POINT('Ctrl Pts',(30.4712297362926,50.16247038998,70.9317462364045)) ;
#6512 = CARTESIAN_POINT('Ctrl Pts',(30.345970660066,50.7598968605682,71.2550771835097)) ;
#6513 = CARTESIAN_POINT('Ctrl Pts',(30.1914127009229,51.3573233311564,71.5654714083249)) ;
#6514 = CARTESIAN_POINT('Ctrl Pts',(30.0368547417798,51.9547498017447,71.8758656331401)) ;
#6515 = CARTESIAN_POINT('Ctrl Pts',(29.8543165337321,52.5521762723329,72.170674961581)) ;
#6516 = CARTESIAN_POINT('Ctrl Pts',(29.6717783256843,53.1496027429211,72.465484290022)) ;
#6517 = CARTESIAN_POINT('Ctrl Pts',(29.4628172203617,53.7470292135094,72.7421935128453)) ;
#6518 = CARTESIAN_POINT('Ctrl Pts',(29.2538561150392,54.3444556840976,73.0189027356686)) ;
#6519 = CARTESIAN_POINT('Ctrl Pts',(29.0202548949149,54.9418821546858,73.27515106735)) ;
#6520 = CARTESIAN_POINT('Ctrl Pts',(28.7866536747906,55.5393086252741,73.5313993990315)) ;
#6521 = CARTESIAN_POINT('Ctrl Pts',(28.5304053431091,56.1367350958623,73.7650006191558)) ;
#6522 = CARTESIAN_POINT('Ctrl Pts',(28.2741570114277,56.7341615664505,73.9986018392801)) ;
#6523 = CARTESIAN_POINT('Ctrl Pts',(27.9974477886044,57.3315880370388,74.2075629446027)) ;
#6524 = CARTESIAN_POINT('Ctrl Pts',(27.7539946265433,57.8572133193466,74.3914102385941)) ;
#6525 = CARTESIAN_POINT('Ctrl Pts',(27.4964139865824,58.3830758086166,74.5548773103327)) ;
#6526 = CARTESIAN_POINT('Ctrl Pts',(58.4776880157526,45.3830502402145,68.2224110288131)) ;
#6527 = CARTESIAN_POINT('Ctrl Pts',(58.4776890657616,45.980480894371,69.8405700656033)) ;
#6528 = CARTESIAN_POINT('Ctrl Pts',(58.3283841860862,46.5779115664505,71.4518263212164)) ;
#6529 = CARTESIAN_POINT('Ctrl Pts',(58.1790803564124,47.1753380370388,73.0630712455076)) ;
#6530 = CARTESIAN_POINT('Ctrl Pts',(57.8817465046965,47.772764507627,74.6536668635808)) ;
#6531 = CARTESIAN_POINT('Ctrl Pts',(57.5844126529807,48.3701909782152,76.2442624816539)) ;
#6532 = CARTESIAN_POINT('Ctrl Pts',(57.1415855268086,48.9676174488035,77.8006383925237)) ;
#6533 = CARTESIAN_POINT('Ctrl Pts',(56.6987584006366,49.5650439193917,79.3570143033935)) ;
#6534 = CARTESIAN_POINT('Ctrl Pts',(56.1142160449124,50.16247038998,80.8658920565512)) ;
#6535 = CARTESIAN_POINT('Ctrl Pts',(55.5296736891883,50.7598968605682,82.3747698097088)) ;
#6536 = CARTESIAN_POINT('Ctrl Pts',(54.8084032131872,51.3573233311564,83.8232761921796)) ;
#6537 = CARTESIAN_POINT('Ctrl Pts',(54.0871327371861,51.9547498017447,85.2717825746505)) ;
#6538 = CARTESIAN_POINT('Ctrl Pts',(53.2352877662965,52.5521762723329,86.6475594407083)) ;
#6539 = CARTESIAN_POINT('Ctrl Pts',(52.3834427954069,53.1496027429211,88.023336306766)) ;
#6540 = CARTESIAN_POINT('Ctrl Pts',(51.4082909705684,53.7470292135094,89.3146460132748)) ;
#6541 = CARTESIAN_POINT('Ctrl Pts',(50.4331391457298,54.3444556840976,90.6059557197835)) ;
#6542 = CARTESIAN_POINT('Ctrl Pts',(49.3430001184831,54.9418821546858,91.8017812676303)) ;
#6543 = CARTESIAN_POINT('Ctrl Pts',(48.2528610912363,55.5393086252741,92.9976068154771)) ;
#6544 = CARTESIAN_POINT('Ctrl Pts',(47.0570355433895,56.1367350958623,94.0877458427239)) ;
#6545 = CARTESIAN_POINT('Ctrl Pts',(45.8612099955427,56.7341615664505,95.1778848699707)) ;
#6546 = CARTESIAN_POINT('Ctrl Pts',(44.569900289034,57.3315880370388,96.1530366948092)) ;
#6547 = CARTESIAN_POINT('Ctrl Pts',(43.4337855327491,57.8572133193466,97.010990733436)) ;
#6548 = CARTESIAN_POINT('Ctrl Pts',(42.2317425462647,58.3830758086166,97.7738370682162)) ;
#6549 = CARTESIAN_POINT('',(38.075012827077,58.3353824278239,91.0374682134905)) ;
#6550 = CARTESIAN_POINT('',(27.7402393245935,58.2172712656981,74.7524658824537)) ;
#6551 = CARTESIAN_POINT('Ctrl Pts',(38.075012827077,58.3353824278239,91.0374682134905)) ;
#6552 = CARTESIAN_POINT('Ctrl Pts',(36.6930174593637,58.3308357083915,88.859791972123)) ;
#6553 = CARTESIAN_POINT('Ctrl Pts',(35.1441429605084,58.3244410146232,86.4191562972014)) ;
#6554 = CARTESIAN_POINT('Ctrl Pts',(32.4831083179517,58.3066351812267,82.2260366573432)) ;
#6555 = CARTESIAN_POINT('Ctrl Pts',(29.560342929611,58.2895264404741,77.6204953552679)) ;
#6556 = CARTESIAN_POINT('Ctrl Pts',(27.7402370295205,58.2172696107898,74.7524673806459)) ;
#6557 = CARTESIAN_POINT('Ctrl Pts',(27.7402393245935,58.2172712656981,74.7524658824537)) ;
#6558 = CARTESIAN_POINT('Ctrl Pts',(27.8754462121168,57.9495340002387,74.6642065097652)) ;
#6559 = CARTESIAN_POINT('Ctrl Pts',(28.0078544340238,57.681908404589,74.5717785787589)) ;
#6560 = CARTESIAN_POINT('Ctrl Pts',(28.1371412783914,57.4145313636563,74.4754405303686)) ;
#6561 = CARTESIAN_POINT('Ctrl Pts',(28.2571575918273,57.1663266301653,74.3860104149692)) ;
#6562 = CARTESIAN_POINT('Ctrl Pts',(28.3745205791364,56.9182638872705,74.2931869169747)) ;
#6563 = CARTESIAN_POINT('Ctrl Pts',(28.489080577214,56.6702295478714,74.1970972024028)) ;
#6564 = CARTESIAN_POINT('Ctrl Pts',(28.4979296409396,56.6510704023379,74.189674855843)) ;
#6565 = CARTESIAN_POINT('Ctrl Pts',(28.5067626169521,56.6319118940954,74.1822324995112)) ;
#6566 = CARTESIAN_POINT('Ctrl Pts',(28.5155794125353,56.6127538456679,74.1747702096408)) ;
#6567 = CARTESIAN_POINT('Ctrl Pts',(28.6312140508663,56.3614909032359,74.0769002769485)) ;
#6568 = CARTESIAN_POINT('Ctrl Pts',(28.7440516725572,56.1103350670436,73.9756114424237)) ;
#6569 = CARTESIAN_POINT('Ctrl Pts',(28.8538256281834,55.8590202585562,73.8711333467298)) ;
#6570 = CARTESIAN_POINT('Ctrl Pts',(28.8607788186558,55.8431017310512,73.8645156012417)) ;
#6571 = CARTESIAN_POINT('Ctrl Pts',(28.8677195431166,55.8271830724928,73.857885278296)) ;
#6572 = CARTESIAN_POINT('Ctrl Pts',(28.8746477921954,55.8112643008986,73.8512423838609)) ;
#6573 = CARTESIAN_POINT('Ctrl Pts',(28.9854377430074,55.5567064895583,73.7450155523287)) ;
#6574 = CARTESIAN_POINT('Ctrl Pts',(29.0930908521726,55.3019957844142,73.6355216404124)) ;
#6575 = CARTESIAN_POINT('Ctrl Pts',(29.1975705510464,55.0471908391174,73.5227738207595)) ;
#6576 = CARTESIAN_POINT('Ctrl Pts',(29.202774724961,55.034498906963,73.5171578085745)) ;
#6577 = CARTESIAN_POINT('Ctrl Pts',(29.2079709717293,55.0218058655745,73.5115337104615)) ;
#6578 = CARTESIAN_POINT('Ctrl Pts',(29.2131592267093,55.0091118266697,73.5059016032595)) ;
#6579 = CARTESIAN_POINT('Ctrl Pts',(29.3186566481837,54.7509925981975,73.3913789382059)) ;
#6580 = CARTESIAN_POINT('Ctrl Pts',(29.420791245856,54.4926055130969,73.2736094403093)) ;
#6581 = CARTESIAN_POINT('Ctrl Pts',(29.5191454608939,54.2345762733043,73.1530981676337)) ;
#6582 = CARTESIAN_POINT('Ctrl Pts',(29.5227356562035,54.2251575070004,73.1486991796925)) ;
#6583 = CARTESIAN_POINT('Ctrl Pts',(29.5263211032666,54.2157389752755,73.144296194541)) ;
#6584 = CARTESIAN_POINT('Ctrl Pts',(29.5299017952159,54.2063206495465,73.139889221293)) ;
#6585 = CARTESIAN_POINT('Ctrl Pts',(29.6292306159036,53.9450551732692,73.0176392590708)) ;
#6586 = CARTESIAN_POINT('Ctrl Pts',(29.7248575150048,53.6840579939705,72.8923709682529)) ;
#6587 = CARTESIAN_POINT('Ctrl Pts',(29.8165233971548,53.4230444575825,72.76444089322)) ;
#6588 = CARTESIAN_POINT('Ctrl Pts',(29.8186881695431,53.4168803877749,72.7614197092465)) ;
#6589 = CARTESIAN_POINT('Ctrl Pts',(29.8208507289346,53.4107163827,72.758397056665)) ;
#6590 = CARTESIAN_POINT('Ctrl Pts',(29.8230110750717,53.4045524432164,72.7553729359249)) ;
#6591 = CARTESIAN_POINT('Ctrl Pts',(29.9156335453573,53.1402803009608,72.6257170772735)) ;
#6592 = CARTESIAN_POINT('Ctrl Pts',(30.0042142732511,52.8760533725719,72.493325654808)) ;
#6593 = CARTESIAN_POINT('Ctrl Pts',(30.0887477381456,52.6118787196959,72.3581998849054)) ;
#6594 = CARTESIAN_POINT('Ctrl Pts',(30.175136346897,52.3419065760271,72.2201086889169)) ;
#6595 = CARTESIAN_POINT('Ctrl Pts',(30.2572393512457,52.0715787920594,72.0792347687965)) ;
#6596 = CARTESIAN_POINT('Ctrl Pts',(30.3348641568369,51.8011908422986,71.9358954676151)) ;
#6597 = CARTESIAN_POINT('Ctrl Pts',(30.3349616095944,51.8008513882913,71.9357155146984)) ;
#6598 = CARTESIAN_POINT('Ctrl Pts',(30.3350590552918,51.8005119341973,71.9355355579006)) ;
#6599 = CARTESIAN_POINT('Ctrl Pts',(30.3351564939286,51.8001724800173,71.9353555972221)) ;
#6600 = CARTESIAN_POINT('Ctrl Pts',(30.4118392607038,51.5330270582815,71.7937292035196)) ;
#6601 = CARTESIAN_POINT('Ctrl Pts',(30.4842968674352,51.2655853544539,71.6493926137567)) ;
#6602 = CARTESIAN_POINT('Ctrl Pts',(30.552072420951,50.998401550286,71.503248573748)) ;
#6603 = CARTESIAN_POINT('Ctrl Pts',(30.5529834678514,50.9948100344075,71.5012840885058)) ;
#6604 = CARTESIAN_POINT('Ctrl Pts',(30.5538936734284,50.991218547496,71.499319267114)) ;
#6605 = CARTESIAN_POINT('Ctrl Pts',(30.5548030365843,50.9876270907846,71.4973541116952)) ;
#6606 = CARTESIAN_POINT('Ctrl Pts',(30.6216299293917,50.723699647588,71.3529396061481)) ;
#6607 = CARTESIAN_POINT('Ctrl Pts',(30.6839607896437,50.4599498020534,71.2066569873818)) ;
#6608 = CARTESIAN_POINT('Ctrl Pts',(30.7418017309264,50.1963788513667,71.0585096581505)) ;
#6609 = CARTESIAN_POINT('Ctrl Pts',(30.7432971955163,50.1895642834339,71.0546793421142)) ;
#6610 = CARTESIAN_POINT('Ctrl Pts',(30.7447896214764,50.1827500045963,71.0508478748386)) ;
#6611 = CARTESIAN_POINT('Ctrl Pts',(30.746279010706,50.175936008737,71.0470152531297)) ;
#6612 = CARTESIAN_POINT('Ctrl Pts',(30.8031794696593,49.9156148757636,70.9005942035517)) ;
#6613 = CARTESIAN_POINT('Ctrl Pts',(30.8555919805957,49.6552611188171,70.7526177854089)) ;
#6614 = CARTESIAN_POINT('Ctrl Pts',(30.9035138752949,49.3948957256021,70.6031422004369)) ;
#6615 = CARTESIAN_POINT('Ctrl Pts',(30.90537060004,49.3848079176934,70.5973507971724)) ;
#6616 = CARTESIAN_POINT('Ctrl Pts',(30.9072205375093,49.3747203101763,70.5915572664575)) ;
#6617 = CARTESIAN_POINT('Ctrl Pts',(30.9090636830444,49.3646329259559,70.5857616238384)) ;
#6618 = CARTESIAN_POINT('Ctrl Pts',(30.9560371523614,49.1075509841657,70.4380568248653)) ;
#6619 = CARTESIAN_POINT('Ctrl Pts',(30.9986538215556,48.8504690628026,70.2887840081728)) ;
#6620 = CARTESIAN_POINT('Ctrl Pts',(31.0367725700753,48.5931578990174,70.1383929388844)) ;
#6621 = CARTESIAN_POINT('Ctrl Pts',(31.0387501111437,48.5798089981879,70.1305908853705)) ;
#6622 = CARTESIAN_POINT('Ctrl Pts',(31.040715607705,48.5664590689811,70.1227855817124)) ;
#6623 = CARTESIAN_POINT('Ctrl Pts',(31.0426690346055,48.553108105864,70.1149771058549)) ;
#6624 = CARTESIAN_POINT('Ctrl Pts',(31.0798470008467,48.2990102146502,69.9663648123762)) ;
#6625 = CARTESIAN_POINT('Ctrl Pts',(31.1126813517942,48.0446012919295,69.8165063124975)) ;
#6626 = CARTESIAN_POINT('Ctrl Pts',(31.1410716961609,47.7903648312086,69.6657693769311)) ;
#6627 = CARTESIAN_POINT('Ctrl Pts',(31.142923648441,47.7737805380755,69.6559365405302)) ;
#6628 = CARTESIAN_POINT('Ctrl Pts',(31.1447567589066,47.7571963611374,69.6460996001179)) ;
#6629 = CARTESIAN_POINT('Ctrl Pts',(31.1465710087748,47.7406123516808,69.6362586086441)) ;
#6630 = CARTESIAN_POINT('Ctrl Pts',(31.1740304610611,47.4896062337396,69.4873109688723)) ;
#6631 = CARTESIAN_POINT('Ctrl Pts',(31.1971065359107,47.2387261489801,69.3378286203306)) ;
#6632 = CARTESIAN_POINT('Ctrl Pts',(31.2158269587204,46.9878897404752,69.1877652509507)) ;
#6633 = CARTESIAN_POINT('Ctrl Pts',(31.217300311963,46.9681481652134,69.1759548151439)) ;
#6634 = CARTESIAN_POINT('Ctrl Pts',(31.218746628802,46.9484074501539,69.1641411312535)) ;
#6635 = CARTESIAN_POINT('Ctrl Pts',(31.2201659213531,46.9286675886395,69.152324196894)) ;
#6636 = CARTESIAN_POINT('Ctrl Pts',(31.2379716343071,46.6810214584577,69.0040750279415)) ;
#6637 = CARTESIAN_POINT('Ctrl Pts',(31.2515255162978,46.4334531760662,68.8552127523791)) ;
#6638 = CARTESIAN_POINT('Ctrl Pts',(31.2607899566468,46.1857600468478,68.70614811867)) ;
#6639 = CARTESIAN_POINT('Ctrl Pts',(31.2616415494885,46.1629919477682,68.6924460092887)) ;
#6640 = CARTESIAN_POINT('Ctrl Pts',(31.2624569163218,46.1402223084086,68.678741898586)) ;
#6641 = CARTESIAN_POINT('Ctrl Pts',(31.2632360228334,46.1174510138863,68.6650361315705)) ;
#6642 = CARTESIAN_POINT('Ctrl Pts',(31.271608391925,45.8727480373429,68.517752366864)) ;
#6643 = CARTESIAN_POINT('Ctrl Pts',(31.2758073873136,45.6279743432133,68.3701949493187)) ;
#6644 = CARTESIAN_POINT('Ctrl Pts',(31.2758081909614,45.3830610445957,68.222429730099)) ;
#6645 = CARTESIAN_POINT('',(57.4106193181313,48.5844537758935,76.7989233032516)) ;
#6646 = CARTESIAN_POINT('Ctrl Pts',(51.7933248065259,45.3830586252741,68.2224337400008)) ;
#6647 = CARTESIAN_POINT('Ctrl Pts',(52.308018473855,45.4231928758842,68.3103779261485)) ;
#6648 = CARTESIAN_POINT('Ctrl Pts',(52.8090405407003,45.4870033972977,68.4552855869039)) ;
#6649 = CARTESIAN_POINT('Ctrl Pts',(53.7748388026689,45.6539797372435,68.8542815132844)) ;
#6650 = CARTESIAN_POINT('Ctrl Pts',(54.2353699749147,45.7573388893141,69.1091189365817)) ;
#6651 = CARTESIAN_POINT('Ctrl Pts',(55.4095055664222,46.0833507061677,69.9408962356853)) ;
#6652 = CARTESIAN_POINT('Ctrl Pts',(56.0396012667916,46.333687722769,70.6083832653474)) ;
#6653 = CARTESIAN_POINT('Ctrl Pts',(57.0466870536474,46.9107591797132,72.1931483430176)) ;
#6654 = CARTESIAN_POINT('Ctrl Pts',(57.3887715545277,47.2383195349501,73.1130504687389)) ;
#6655 = CARTESIAN_POINT('Ctrl Pts',(57.673423309298,47.9083523080808,74.9787376424982)) ;
#6656 = CARTESIAN_POINT('Ctrl Pts',(57.6305961076901,48.2450338483643,75.907165158477)) ;
#6657 = CARTESIAN_POINT('Ctrl Pts',(57.4106193181313,48.5844537758935,76.7989233032516)) ;
#6658 = CARTESIAN_POINT('',(57.3984019004021,48.6029307720944,76.8474073371282)) ;
#6659 = CARTESIAN_POINT('Origin',(92.1683318818475,48.3646139793373,85.6889926784978)) ;
#6660 = CARTESIAN_POINT('',(49.1121349038258,55.0677871747466,92.0526694236409)) ;
#6661 = CARTESIAN_POINT('Ctrl Pts',(57.3984019004021,48.6029307720944,76.8474073371282)) ;
#6662 = CARTESIAN_POINT('Ctrl Pts',(57.2766816661225,48.785356686239,77.3258247136573)) ;
#6663 = CARTESIAN_POINT('Ctrl Pts',(57.1415855268086,48.9676174488035,77.8006383925237)) ;
#6664 = CARTESIAN_POINT('Ctrl Pts',(56.6987584006366,49.5650439193917,79.3570143033935)) ;
#6665 = CARTESIAN_POINT('Ctrl Pts',(56.1142160449124,50.16247038998,80.8658920565512)) ;
#6666 = CARTESIAN_POINT('Ctrl Pts',(55.5296736891883,50.7598968605682,82.3747698097088)) ;
#6667 = CARTESIAN_POINT('Ctrl Pts',(54.8084032131872,51.3573233311564,83.8232761921796)) ;
#6668 = CARTESIAN_POINT('Ctrl Pts',(54.0871327371861,51.9547498017447,85.2717825746505)) ;
#6669 = CARTESIAN_POINT('Ctrl Pts',(53.2352877662965,52.5521762723329,86.6475594407083)) ;
#6670 = CARTESIAN_POINT('Ctrl Pts',(52.3834427954069,53.1496027429211,88.023336306766)) ;
#6671 = CARTESIAN_POINT('Ctrl Pts',(51.4082909705684,53.7470292135094,89.3146460132748)) ;
#6672 = CARTESIAN_POINT('Ctrl Pts',(50.4331391457298,54.3444556840976,90.6059557197835)) ;
#6673 = CARTESIAN_POINT('Ctrl Pts',(49.3430001184831,54.9418821546858,91.8017812676303)) ;
#6674 = CARTESIAN_POINT('Ctrl Pts',(49.2281522354556,55.0048219850164,91.9277633939534)) ;
#6675 = CARTESIAN_POINT('Ctrl Pts',(49.1121349038258,55.0677871747466,92.0526694236409)) ;
#6676 = CARTESIAN_POINT('',(49.0780136113479,55.0862551252693,92.0892167113166)) ;
#6677 = CARTESIAN_POINT('Origin',(75.4923509619182,55.5526174178892,116.574769538313)) ;
#6678 = CARTESIAN_POINT('Ctrl Pts',(49.0780136113479,55.0862551252693,92.0892167113166)) ;
#6679 = CARTESIAN_POINT('Ctrl Pts',(48.7067240185058,55.2861476427455,92.4829396223812)) ;
#6680 = CARTESIAN_POINT('Ctrl Pts',(48.2907363800878,55.4856144064204,92.8325865509095)) ;
#6681 = CARTESIAN_POINT('Ctrl Pts',(47.3532876815545,55.8948727823201,93.4506135013496)) ;
#6682 = CARTESIAN_POINT('Ctrl Pts',(46.8292280164247,56.1030297966033,93.709526588545)) ;
#6683 = CARTESIAN_POINT('Ctrl Pts',(45.3720572721415,56.6395229540349,94.2145561773987)) ;
#6684 = CARTESIAN_POINT('Ctrl Pts',(44.4045376611851,56.955307721454,94.3415217577794)) ;
#6685 = CARTESIAN_POINT('Ctrl Pts',(42.541193176401,57.5027528833962,94.1944856565899)) ;
#6686 = CARTESIAN_POINT('Ctrl Pts',(41.6597611935,57.735639297119,93.9520695669813)) ;
#6687 = CARTESIAN_POINT('Ctrl Pts',(40.24270309089,58.0583687617077,93.2401772744575)) ;
#6688 = CARTESIAN_POINT('Ctrl Pts',(39.6843220177388,58.1679507457141,92.8513543260053)) ;
#6689 = CARTESIAN_POINT('Ctrl Pts',(38.7635710417162,58.3023925284601,91.9849192838713)) ;
#6690 = CARTESIAN_POINT('Ctrl Pts',(38.3891340647941,58.3364158763933,91.5324440811863)) ;
#6691 = CARTESIAN_POINT('Ctrl Pts',(38.075012827077,58.3353824278239,91.0374682134905)) ;
#6692 = CARTESIAN_POINT('Ctrl Pts',(58.4776880737725,45.3830585852922,68.1224336317086)) ;
#6693 = CARTESIAN_POINT('Ctrl Pts',(58.482311357954,45.9804850758286,69.7405813455768)) ;
#6694 = CARTESIAN_POINT('Ctrl Pts',(58.3376110801056,46.5779115664505,71.3522529089681)) ;
#6695 = CARTESIAN_POINT('Ctrl Pts',(58.1929108071096,47.1753380370388,72.9639244183148)) ;
#6696 = CARTESIAN_POINT('Ctrl Pts',(57.9001215138071,47.772764507627,74.555369564329)) ;
#6697 = CARTESIAN_POINT('Ctrl Pts',(57.6073322205045,48.3701909782153,76.1468147103432)) ;
#6698 = CARTESIAN_POINT('Ctrl Pts',(57.1689518819114,48.9676174488035,77.704455844167)) ;
#6699 = CARTESIAN_POINT('Ctrl Pts',(56.7305715433182,49.5650439193917,79.2620969779907)) ;
#6700 = CARTESIAN_POINT('Ctrl Pts',(56.1503402659147,50.16247038998,80.772644854679)) ;
#6701 = CARTESIAN_POINT('Ctrl Pts',(55.5701089885112,50.7598968605682,82.2831927313673)) ;
#6702 = CARTESIAN_POINT('Ctrl Pts',(54.8529771009725,51.3573233311564,83.7337598890405)) ;
#6703 = CARTESIAN_POINT('Ctrl Pts',(54.1358452134337,51.9547498017447,85.1843270467136)) ;
#6704 = CARTESIAN_POINT('Ctrl Pts',(53.2879310321705,52.5521762723329,86.5625377578378)) ;
#6705 = CARTESIAN_POINT('Ctrl Pts',(52.4400168509074,53.1496027429211,87.9407484689621)) ;
#6706 = CARTESIAN_POINT('Ctrl Pts',(51.4685544807482,53.7470292135094,89.2348443256936)) ;
#6707 = CARTESIAN_POINT('Ctrl Pts',(50.497092110589,54.3444556840976,90.5289401824251)) ;
#6708 = CARTESIAN_POINT('Ctrl Pts',(49.4103697259481,54.9418821546858,91.7278804151995)) ;
#6709 = CARTESIAN_POINT('Ctrl Pts',(48.3236473413072,55.5393086252741,92.9268206479739)) ;
#6710 = CARTESIAN_POINT('Ctrl Pts',(47.1309364744028,56.1367350958623,94.0203763214597)) ;
#6711 = CARTESIAN_POINT('Ctrl Pts',(45.9382256074983,56.7341615664505,95.1139319949454)) ;
#6712 = CARTESIAN_POINT('Ctrl Pts',(44.6497020469088,57.3315880370388,96.0927732777132)) ;
#6713 = CARTESIAN_POINT('Ctrl Pts',(43.5159923066831,57.8572347768351,96.9540085165172)) ;
#6714 = CARTESIAN_POINT('Ctrl Pts',(42.3160773566393,58.3831186720347,97.7203165644338)) ;
#6715 = CARTESIAN_POINT('Ctrl Pts',(30.9776880154505,45.3830585852922,68.1224337167953)) ;
#6716 = CARTESIAN_POINT('Ctrl Pts',(30.9823112956982,45.9804850758286,68.4691796548923)) ;
#6717 = CARTESIAN_POINT('Ctrl Pts',(30.954921173919,46.5779115664506,68.8148730183461)) ;
#6718 = CARTESIAN_POINT('Ctrl Pts',(30.9275310530584,47.1753380370388,69.1605663702075)) ;
#6719 = CARTESIAN_POINT('Ctrl Pts',(30.8683612151709,47.772764507627,69.5022578136567)) ;
#6720 = CARTESIAN_POINT('Ctrl Pts',(30.8091913772834,48.3701909782152,69.8439492571058)) ;
#6721 = CARTESIAN_POINT('Ctrl Pts',(30.7187466385633,48.9676174488035,70.1787236012241)) ;
#6722 = CARTESIAN_POINT('Ctrl Pts',(30.6283018998432,49.5650439193917,70.5134979453425)) ;
#6723 = CARTESIAN_POINT('Ctrl Pts',(30.5073539029114,50.16247038998,70.838499013464)) ;
#6724 = CARTESIAN_POINT('Ctrl Pts',(30.3864059059795,50.7598968605682,71.1635000815856)) ;
#6725 = CARTESIAN_POINT('Ctrl Pts',(30.2359865365006,51.3573233311564,71.4759550791893)) ;
#6726 = CARTESIAN_POINT('Ctrl Pts',(30.0855671670217,51.9547498017447,71.7884100767931)) ;
#6727 = CARTESIAN_POINT('Ctrl Pts',(29.9069597500198,52.5521762723329,72.085653248008)) ;
#6728 = CARTESIAN_POINT('Ctrl Pts',(29.7283523330179,53.1496027429211,72.3828964192229)) ;
#6729 = CARTESIAN_POINT('Ctrl Pts',(29.5230806839997,53.7470292135094,72.6623917901172)) ;
#6730 = CARTESIAN_POINT('Ctrl Pts',(29.3178090349815,54.3444556840976,72.9418871610115)) ;
#6731 = CARTESIAN_POINT('Ctrl Pts',(29.0876244592796,54.9418821546858,73.2012501756279)) ;
#6732 = CARTESIAN_POINT('Ctrl Pts',(28.8574398835777,55.5393086252741,73.4606131902444)) ;
#6733 = CARTESIAN_POINT('Ctrl Pts',(28.6043062348312,56.1367350958623,73.6976310547911)) ;
#6734 = CARTESIAN_POINT('Ctrl Pts',(28.3511725860848,56.7341615664505,73.9346489193378)) ;
#6735 = CARTESIAN_POINT('Ctrl Pts',(28.0772495113324,57.3315880370388,74.1472994809647)) ;
#6736 = CARTESIAN_POINT('Ctrl Pts',(27.8362378081571,57.857234776835,74.3344004547882)) ;
#6737 = CARTESIAN_POINT('Ctrl Pts',(27.5808257495764,58.3831186720347,74.5013079016107)) ;
#6738 = CARTESIAN_POINT('',(27.7390441888434,58.3830537363181,74.7506193750977)) ;
#6739 = CARTESIAN_POINT('Ctrl Pts',(31.2729697953901,45.3830674541112,68.1224191093439)) ;
#6740 = CARTESIAN_POINT('Ctrl Pts',(31.2731002040288,45.3999249614352,68.1325854719125)) ;
#6741 = CARTESIAN_POINT('Ctrl Pts',(31.2732122621832,45.4170195560987,68.1428947122456)) ;
#6742 = CARTESIAN_POINT('Ctrl Pts',(31.2733941703955,45.4509660823354,68.1633665015427)) ;
#6743 = CARTESIAN_POINT('Ctrl Pts',(31.2734649447084,45.467937485669,68.1736011010902)) ;
#6744 = CARTESIAN_POINT('Ctrl Pts',(31.2736167856114,45.5188462146266,68.2043008651703)) ;
#6745 = CARTESIAN_POINT('Ctrl Pts',(31.2736373705305,45.5527780591987,68.224761995133)) ;
#6746 = CARTESIAN_POINT('Ctrl Pts',(31.2734576427624,45.6545524513432,68.2861280505301)) ;
#6747 = CARTESIAN_POINT('Ctrl Pts',(31.2730158320587,45.7223738576057,68.3270156411209)) ;
#6748 = CARTESIAN_POINT('Ctrl Pts',(31.2712928003503,45.8755455989765,68.4193346417184)) ;
#6749 = CARTESIAN_POINT('Ctrl Pts',(31.2698234610056,45.9608834226846,68.4707523146004)) ;
#6750 = CARTESIAN_POINT('Ctrl Pts',(31.2666852108686,46.0963466756237,68.5523307651114)) ;
#6751 = CARTESIAN_POINT('Ctrl Pts',(31.2653472956213,46.1464973799214,68.5825318896186)) ;
#6752 = CARTESIAN_POINT('Ctrl Pts',(31.2568446873907,46.4282028809672,68.7521513571258)) ;
#6753 = CARTESIAN_POINT('Ctrl Pts',(31.2461154561705,46.6594344485716,68.8912820844549)) ;
#6754 = CARTESIAN_POINT('Ctrl Pts',(31.2292419752858,46.9296827699017,69.053312093353)) ;
#6755 = CARTESIAN_POINT('Ctrl Pts',(31.2266938785506,46.9687950424149,69.0767488265404)) ;
#6756 = CARTESIAN_POINT('Ctrl Pts',(31.2076132849116,47.2499758749323,69.2451407456555)) ;
#6757 = CARTESIAN_POINT('Ctrl Pts',(31.187138450914,47.4918541916759,69.3894818460527)) ;
#6758 = CARTESIAN_POINT('Ctrl Pts',(31.134152559873,48.0143150857869,69.7001535512841)) ;
#6759 = CARTESIAN_POINT('Ctrl Pts',(31.1002399082149,48.2952954282261,69.8661264207476)) ;
#6760 = CARTESIAN_POINT('Ctrl Pts',(31.0586022138039,48.5931204307081,70.0407394220474)) ;
#6761 = CARTESIAN_POINT('Ctrl Pts',(31.0562056645437,48.6101204742725,70.0507024497919)) ;
#6762 = CARTESIAN_POINT('Ctrl Pts',(31.0162768638686,48.891036215033,70.2152669033389)) ;
#6763 = CARTESIAN_POINT('Ctrl Pts',(30.97399601099,49.1549226796806,70.3688528007291)) ;
#6764 = CARTESIAN_POINT('Ctrl Pts',(30.926014393781,49.4249376060053,70.5243549547346)) ;
#6765 = CARTESIAN_POINT('Ctrl Pts',(30.9249701498923,49.4308011237537,70.5277310753253)) ;
#6766 = CARTESIAN_POINT('Ctrl Pts',(30.8757301114589,49.7066812295574,70.6865457989593)) ;
#6767 = CARTESIAN_POINT('Ctrl Pts',(30.8226320620207,49.9768666464287,70.8406088060635)) ;
#6768 = CARTESIAN_POINT('Ctrl Pts',(30.763508756557,50.2527043291673,70.996102876115)) ;
#6769 = CARTESIAN_POINT('Ctrl Pts',(30.7623588146578,50.2580605419639,70.9991215703048)) ;
#6770 = CARTESIAN_POINT('Ctrl Pts',(30.7041887220664,50.5285623062296,71.1515381204764)) ;
#6771 = CARTESIAN_POINT('Ctrl Pts',(30.6425647115896,50.794089282034,71.2992229922643)) ;
#6772 = CARTESIAN_POINT('Ctrl Pts',(30.572121971017,51.0767673302899,71.4543847718665)) ;
#6773 = CARTESIAN_POINT('Ctrl Pts',(30.5679317898639,51.0935097128498,71.4635669735966)) ;
#6774 = CARTESIAN_POINT('Ctrl Pts',(30.5281873953612,51.2516332986662,71.5502158138466)) ;
#6775 = CARTESIAN_POINT('Ctrl Pts',(30.4913068609656,51.3931664825954,71.6272604837886)) ;
#6776 = CARTESIAN_POINT('Ctrl Pts',(30.4227007802738,51.6479675595822,71.764730378545)) ;
#6777 = CARTESIAN_POINT('Ctrl Pts',(30.3914137616775,51.7612319406863,71.8254116450958)) ;
#6778 = CARTESIAN_POINT('Ctrl Pts',(30.3513694705723,51.9026374456283,71.9006379050749)) ;
#6779 = CARTESIAN_POINT('Ctrl Pts',(30.3433428020212,51.9308091085123,71.9155985690478)) ;
#6780 = CARTESIAN_POINT('Ctrl Pts',(30.254218376761,52.2417252333148,72.0804209027061)) ;
#6781 = CARTESIAN_POINT('Ctrl Pts',(30.1682727980748,52.524119549272,72.2276169079598)) ;
#6782 = CARTESIAN_POINT('Ctrl Pts',(30.0033152730407,53.0381974993267,72.4899907921184)) ;
#6783 = CARTESIAN_POINT('Ctrl Pts',(29.9259031671205,53.2697333986821,72.6060846287223)) ;
#6784 = CARTESIAN_POINT('Ctrl Pts',(29.8276482002984,53.5522259966914,72.7451927295007)) ;
#6785 = CARTESIAN_POINT('Ctrl Pts',(29.8097755308276,53.6031771340237,72.7701819457636)) ;
#6786 = CARTESIAN_POINT('Ctrl Pts',(29.7138859105828,53.8742457620993,72.9025930757515)) ;
#6787 = CARTESIAN_POINT('Ctrl Pts',(29.6332371813762,54.0945463050599,73.0081686491436)) ;
#6788 = CARTESIAN_POINT('Ctrl Pts',(29.526309645954,54.3774106831913,73.1409687184945)) ;
#6789 = CARTESIAN_POINT('Ctrl Pts',(29.5024838913393,54.4398806254194,73.1701248283594)) ;
#6790 = CARTESIAN_POINT('Ctrl Pts',(29.398005894515,54.7114321392953,73.2961024622914)) ;
#6791 = CARTESIAN_POINT('Ctrl Pts',(29.3151050184895,54.9205828276713,73.3912609624358)) ;
#6792 = CARTESIAN_POINT('Ctrl Pts',(29.200017146324,55.203368432956,73.5170824558052)) ;
#6793 = CARTESIAN_POINT('Ctrl Pts',(29.1696780956447,55.2772338818111,73.5496854174052)) ;
#6794 = CARTESIAN_POINT('Ctrl Pts',(29.0572712397692,55.5485088102172,73.6684197231037)) ;
#6795 = CARTESIAN_POINT('Ctrl Pts',(28.9735572714829,55.7457837763595,73.752890529924)) ;
#6796 = CARTESIAN_POINT('Ctrl Pts',(28.85093682095,56.0282588904742,73.8710838626765)) ;
#6797 = CARTESIAN_POINT('Ctrl Pts',(28.8135798522358,56.1134884206095,73.9063851924763)) ;
#6798 = CARTESIAN_POINT('Ctrl Pts',(28.6936894265498,56.3844426291116,74.0174544380719)) ;
#6799 = CARTESIAN_POINT('Ctrl Pts',(28.6099617745652,56.5701302611217,74.0917343757168)) ;
#6800 = CARTESIAN_POINT('Ctrl Pts',(28.4801870114973,56.8526653482997,74.20196576487)) ;
#6801 = CARTESIAN_POINT('Ctrl Pts',(28.4352967717226,56.9494716030796,74.2392362716071)) ;
#6802 = CARTESIAN_POINT('Ctrl Pts',(28.3084560784753,57.220441360115,74.3421652352563)) ;
#6803 = CARTESIAN_POINT('Ctrl Pts',(28.2255259009952,57.3946576755337,74.4067251242961)) ;
#6804 = CARTESIAN_POINT('Ctrl Pts',(28.0888919857564,57.6774250653642,74.5087254230024)) ;
#6805 = CARTESIAN_POINT('Ctrl Pts',(28.0359724099055,57.7859396412659,74.5472038149203)) ;
#6806 = CARTESIAN_POINT('Ctrl Pts',(27.9692360255816,57.9216227418851,74.5944549811629)) ;
#6807 = CARTESIAN_POINT('Ctrl Pts',(27.9558731511316,57.9487278912592,74.603853248453)) ;
#6808 = CARTESIAN_POINT('Ctrl Pts',(27.9089544007098,58.0436810159811,74.6366316934481)) ;
#6809 = CARTESIAN_POINT('Ctrl Pts',(27.8752324837114,58.1115399743052,74.6597974493204)) ;
#6810 = CARTESIAN_POINT('Ctrl Pts',(27.8243671241468,58.2133484522819,74.6941541076358)) ;
#6811 = CARTESIAN_POINT('Ctrl Pts',(27.8073663790787,58.2472850649056,74.7055400425132)) ;
#6812 = CARTESIAN_POINT('Ctrl Pts',(27.7817951862796,58.2981973836578,74.722520540854)) ;
#6813 = CARTESIAN_POINT('Ctrl Pts',(27.7732597760152,58.3151693899102,74.7281643060626)) ;
#6814 = CARTESIAN_POINT('Ctrl Pts',(27.762384280287,58.3367668565644,74.7353246686243)) ;
#6815 = CARTESIAN_POINT('Ctrl Pts',(27.7600504741546,58.3413999128692,74.736859442133)) ;
#6816 = CARTESIAN_POINT('Ctrl Pts',(27.7514785817235,58.3584108602027,74.742489946245)) ;
#6817 = CARTESIAN_POINT('Ctrl Pts',(27.7452310605373,58.3707975233385,74.7465807676633)) ;
#6818 = CARTESIAN_POINT('Ctrl Pts',(27.7390451836026,58.3830508753326,74.7506187222499)) ;
#6819 = CARTESIAN_POINT('',(38.075012827077,58.3831162793798,91.0374682134904)) ;
#6820 = CARTESIAN_POINT('Ctrl Pts',(27.739058487419,58.3830900980199,74.7506102954531)) ;
#6821 = CARTESIAN_POINT('Ctrl Pts',(29.4617175445255,58.3831052593851,77.4650866159089)) ;
#6822 = CARTESIAN_POINT('Ctrl Pts',(31.1843766016598,58.3831073991803,80.1795629364082)) ;
#6823 = CARTESIAN_POINT('Ctrl Pts',(34.6296947148817,58.3831134572106,85.6085155757581)) ;
#6824 = CARTESIAN_POINT('Ctrl Pts',(36.3523537709793,58.383115023513,88.3229918946244)) ;
#6825 = CARTESIAN_POINT('Ctrl Pts',(38.0750128270769,58.3831162793798,91.0374682134904)) ;
#6826 = CARTESIAN_POINT('',(49.11218721881,55.104724217109,92.0527180565764)) ;
#6827 = CARTESIAN_POINT('Ctrl Pts',(38.075012827077,58.3831162793798,91.0374682134904)) ;
#6828 = CARTESIAN_POINT('Ctrl Pts',(38.3910170362888,58.3831165097557,91.535411169487)) ;
#6829 = CARTESIAN_POINT('Ctrl Pts',(38.7680285100977,58.3477204189414,91.990287868787)) ;
#6830 = CARTESIAN_POINT('Ctrl Pts',(39.6959726062055,58.2097833704152,92.8609217685079)) ;
#6831 = CARTESIAN_POINT('Ctrl Pts',(40.2592080825518,58.0979491851445,93.251035058612)) ;
#6832 = CARTESIAN_POINT('Ctrl Pts',(41.6832452702688,57.7707078254697,93.9602870316529)) ;
#6833 = CARTESIAN_POINT('Ctrl Pts',(42.5660592155094,57.5360202457533,94.199694127608)) ;
#6834 = CARTESIAN_POINT('Ctrl Pts',(44.4307136974944,56.9856758817168,94.3399656139212)) ;
#6835 = CARTESIAN_POINT('Ctrl Pts',(45.3981702829227,56.6687344805943,94.2093431307212)) ;
#6836 = CARTESIAN_POINT('Ctrl Pts',(46.8577625330414,56.1294192803767,93.6971962023311)) ;
#6837 = CARTESIAN_POINT('Ctrl Pts',(47.384386064077,55.9194276565171,93.4339192562471)) ;
#6838 = CARTESIAN_POINT('Ctrl Pts',(48.3247863893035,55.5068628236253,92.8063316588796)) ;
#6839 = CARTESIAN_POINT('Ctrl Pts',(48.7412751267391,55.3059550653476,92.4517122776391)) ;
#6840 = CARTESIAN_POINT('Ctrl Pts',(49.11218721881,55.104724217109,92.0527180565764)) ;
#6841 = CARTESIAN_POINT('',(57.3984711260663,48.6398835186857,76.8474249390433)) ;
#6842 = CARTESIAN_POINT('Ctrl Pts',(57.3984711260663,48.6398835186857,76.8474249390432)) ;
#6843 = CARTESIAN_POINT('Ctrl Pts',(57.2891432146506,48.8038201453524,77.2773950439918)) ;
#6844 = CARTESIAN_POINT('Ctrl Pts',(57.1689518258159,48.9676174488035,77.7044558282064)) ;
#6845 = CARTESIAN_POINT('Ctrl Pts',(56.7305714879606,49.5650439193917,79.2620969594367)) ;
#6846 = CARTESIAN_POINT('Ctrl Pts',(56.1503402115311,50.16247038998,80.7726448336107)) ;
#6847 = CARTESIAN_POINT('Ctrl Pts',(55.5701089351017,50.7598968605682,82.2831927077847)) ;
#6848 = CARTESIAN_POINT('Ctrl Pts',(54.8529770487648,51.3573233311564,83.7337598630442)) ;
#6849 = CARTESIAN_POINT('Ctrl Pts',(54.1358451624279,51.9547498017447,85.1843270183036)) ;
#6850 = CARTESIAN_POINT('Ctrl Pts',(53.2879309825842,52.5521762723329,86.5625377271353)) ;
#6851 = CARTESIAN_POINT('Ctrl Pts',(52.4400168027405,53.1496027429211,87.9407484359671)) ;
#6852 = CARTESIAN_POINT('Ctrl Pts',(51.4685544342063,53.7470292135094,89.2348442905468)) ;
#6853 = CARTESIAN_POINT('Ctrl Pts',(50.4970920656721,54.3444556840976,90.5289401451265)) ;
#6854 = CARTESIAN_POINT('Ctrl Pts',(49.4103696828477,54.9418821546858,91.7278803759083)) ;
#6855 = CARTESIAN_POINT('Ctrl Pts',(49.262301577525,55.0232827101246,91.8912383881963)) ;
#6856 = CARTESIAN_POINT('Ctrl Pts',(49.11218721881,55.104724217109,92.0527180565764)) ;
#6857 = CARTESIAN_POINT('Ctrl Pts',(57.3984711260663,48.6398835186857,76.8474249390433)) ;
#6858 = CARTESIAN_POINT('Ctrl Pts',(57.5318809087092,48.4398362531007,76.3227444846068)) ;
#6859 = CARTESIAN_POINT('Ctrl Pts',(57.6040805147783,48.2402511664186,75.7839347717915)) ;
#6860 = CARTESIAN_POINT('Ctrl Pts',(57.6232176241361,47.8311033708304,74.6615809415638)) ;
#6861 = CARTESIAN_POINT('Ctrl Pts',(57.5609538539119,47.6231195575042,74.0809852902915)) ;
#6862 = CARTESIAN_POINT('Ctrl Pts',(57.2066131255233,47.0862679673289,72.5806485964983)) ;
#6863 = CARTESIAN_POINT('Ctrl Pts',(56.7952723804051,46.7703269230099,71.6955878783151)) ;
#6864 = CARTESIAN_POINT('Ctrl Pts',(55.6718207466244,46.2216256025066,70.200388721669)) ;
#6865 = CARTESIAN_POINT('Ctrl Pts',(54.9943545947592,45.987905739686,69.5859906898853)) ;
#6866 = CARTESIAN_POINT('Ctrl Pts',(53.6339893980261,45.6640068127921,68.7717169071534)) ;
#6867 = CARTESIAN_POINT('Ctrl Pts',(53.0073921260216,45.5539383581279,68.5091118556871)) ;
#6868 = CARTESIAN_POINT('Ctrl Pts',(51.7834240894348,45.4179657700952,68.1961600284618)) ;
#6869 = CARTESIAN_POINT('Ctrl Pts',(51.2006845491435,45.3830585853871,68.1224336562375)) ;
#6870 = CARTESIAN_POINT('Ctrl Pts',(50.6143411942707,45.3830586252741,68.1224337400008)) ;
#6871 = CARTESIAN_POINT('Origin',(50.6143421942707,45.3822493559848,75.1224337400008)) ;
#6872 = CARTESIAN_POINT('',(57.3984711260663,45.3822493559848,76.8474249390433)) ;
#6873 = CARTESIAN_POINT('Origin',(23.47768801576,45.3822493559848,68.2224337400008)) ;
#6874 = CARTESIAN_POINT('',(49.11218721881,45.3822493559848,92.0527180565764)) ;
#6875 = CARTESIAN_POINT('Origin',(43.9853083041937,45.3822493559848,87.2866806464355)) ;
#6876 = CARTESIAN_POINT('',(38.075012827077,45.3822493559848,91.0374682134905)) ;
#6877 = CARTESIAN_POINT('Origin',(27.5808403303614,45.3822493559848,74.5012983732667)) ;
#6878 = CARTESIAN_POINT('Ctrl Pts',(27.6340699934267,57.8265499701676,74.5851749008597)) ;
#6879 = CARTESIAN_POINT('Ctrl Pts',(27.6340965843113,57.8721147554955,74.585216801389)) ;
#6880 = CARTESIAN_POINT('Ctrl Pts',(27.6363074785453,57.9184467890563,74.5887006131945)) ;
#6881 = CARTESIAN_POINT('Ctrl Pts',(27.6453547210266,58.0066958708245,74.6029567861613)) ;
#6882 = CARTESIAN_POINT('Ctrl Pts',(27.6523019245548,58.0508719524288,74.6139038272942)) ;
#6883 = CARTESIAN_POINT('Ctrl Pts',(27.671671280061,58.1278680023598,74.6444250477569)) ;
#6884 = CARTESIAN_POINT('Ctrl Pts',(27.6828616512215,58.1579990080347,74.6620582511416)) ;
#6885 = CARTESIAN_POINT('Ctrl Pts',(27.7020567681637,58.1911673828821,74.6923049155601)) ;
#6886 = CARTESIAN_POINT('Ctrl Pts',(27.7096119577989,58.201115371274,74.7042099894589)) ;
#6887 = CARTESIAN_POINT('Ctrl Pts',(27.7250554624726,58.2136587167095,74.7285450588789)) ;
#6888 = CARTESIAN_POINT('Ctrl Pts',(27.7325146430327,58.2169692427633,74.740298846674)) ;
#6889 = CARTESIAN_POINT('Ctrl Pts',(27.7402369588892,58.217275807636,74.7524672693487)) ;
#6890 = CARTESIAN_POINT('Ctrl Pts',(27.7390583718472,58.3830247512584,74.7506101133411)) ;
#6891 = CARTESIAN_POINT('Ctrl Pts',(27.7352912521335,58.3830247228386,74.7446740825189)) ;
#6892 = CARTESIAN_POINT('Ctrl Pts',(27.7315547998714,58.3837424765073,74.7387863758678)) ;
#6893 = CARTESIAN_POINT('Ctrl Pts',(27.7239251145917,58.3866521090709,74.726763915626)) ;
#6894 = CARTESIAN_POINT('Ctrl Pts',(27.720097441989,58.3889169428631,74.7207324687187)) ;
#6895 = CARTESIAN_POINT('Ctrl Pts',(27.707904199704,58.398544443072,74.7015189932978)) ;
#6896 = CARTESIAN_POINT('Ctrl Pts',(27.7002505376832,58.4085611720351,74.689458751802)) ;
#6897 = CARTESIAN_POINT('Ctrl Pts',(27.68144026452,58.4411881110121,74.659818504144)) ;
#6898 = CARTESIAN_POINT('Ctrl Pts',(27.6706669109948,58.470179097251,74.6428424153515)) ;
#6899 = CARTESIAN_POINT('Ctrl Pts',(27.6518069653766,58.5450324120644,74.613123896429)) ;
#6900 = CARTESIAN_POINT('Ctrl Pts',(27.645027480032,58.5884045335157,74.6024411370552)) ;
#6901 = CARTESIAN_POINT('Ctrl Pts',(27.6361980719596,58.6752752681755,74.5885282161917)) ;
#6902 = CARTESIAN_POINT('Ctrl Pts',(27.6340701087039,58.7210386854942,74.5851750825074)) ;
#6903 = CARTESIAN_POINT('Ctrl Pts',(27.6340702593408,58.7660385537336,74.5851753198732)) ;
#6904 = CARTESIAN_POINT('Origin',(23.47768801576,43.8830586252741,68.2224337400009)) ;
#6905 = CARTESIAN_POINT('Ctrl Pts',(27.701230891149,58.2943663992286,74.7777638904556)) ;
#6906 = CARTESIAN_POINT('Ctrl Pts',(27.5958999514269,58.2924602039142,74.6121580162595)) ;
#6907 = CARTESIAN_POINT('Ctrl Pts',(27.4526548484823,58.191081348463,74.7000597463983)) ;
#6908 = CARTESIAN_POINT('Ctrl Pts',(27.9760338094669,57.7522999681945,74.6007093188303)) ;
#6909 = CARTESIAN_POINT('Ctrl Pts',(27.8637630679054,57.7503889242577,74.4395201306975)) ;
#6910 = CARTESIAN_POINT('Ctrl Pts',(27.7242147844289,57.6489874075334,74.5334181808899)) ;
#6911 = CARTESIAN_POINT('Ctrl Pts',(28.2392666218688,57.2111033102745,74.4066346294935)) ;
#6912 = CARTESIAN_POINT('Ctrl Pts',(28.120340108254,57.2091968026367,74.2502911525297)) ;
#6913 = CARTESIAN_POINT('Ctrl Pts',(27.9848160276798,57.1078632090985,74.3499766830414)) ;
#6914 = CARTESIAN_POINT('Ctrl Pts',(28.6139877302149,56.3997926693382,74.0923287003896)) ;
#6915 = CARTESIAN_POINT('Ctrl Pts',(28.4855837933368,56.3978864499605,73.9438397893937)) ;
#6916 = CARTESIAN_POINT('Ctrl Pts',(28.3566661229263,56.2965290899915,74.0517406446381)) ;
#6917 = CARTESIAN_POINT('Ctrl Pts',(28.7356674654984,56.1295297083681,73.9835911448773)) ;
#6918 = CARTESIAN_POINT('Ctrl Pts',(28.6041845210826,56.1276240321417,73.8378196428817)) ;
#6919 = CARTESIAN_POINT('Ctrl Pts',(28.4775758252667,56.0262125668428,73.9483736489995)) ;
#6920 = CARTESIAN_POINT('Ctrl Pts',(28.9719840952407,55.5885108130589,73.7586758721593)) ;
#6921 = CARTESIAN_POINT('Ctrl Pts',(28.8345207694355,55.5866055506407,73.6185325946753)) ;
#6922 = CARTESIAN_POINT('Ctrl Pts',(28.7126128644989,55.485272016298,73.7343143425878)) ;
#6923 = CARTESIAN_POINT('Ctrl Pts',(29.0865699779388,55.3179011606642,73.6425604457781)) ;
#6924 = CARTESIAN_POINT('Ctrl Pts',(28.9462064140221,55.3159940909988,73.505321568464)) ;
#6925 = CARTESIAN_POINT('Ctrl Pts',(28.8267510070548,55.2146518759856,73.6236251304476)) ;
#6926 = CARTESIAN_POINT('Ctrl Pts',(29.3085722187904,54.7764805321466,73.4029882220714)) ;
#6927 = CARTESIAN_POINT('Ctrl Pts',(29.1625852444779,54.774572825861,73.2717424098044)) ;
#6928 = CARTESIAN_POINT('Ctrl Pts',(29.0482354201187,54.673110454093,73.3948939802413)) ;
#6929 = CARTESIAN_POINT('Ctrl Pts',(29.4159635790958,54.5052712784355,73.2795250922713)) ;
#6930 = CARTESIAN_POINT('Ctrl Pts',(29.2672561254484,54.5033650628135,73.15137495925)) ;
#6931 = CARTESIAN_POINT('Ctrl Pts',(29.1554659475733,54.4020271817646,73.2769499969672)) ;
#6932 = CARTESIAN_POINT('Ctrl Pts',(29.6223275764867,53.9638812711181,73.0266714360963)) ;
#6933 = CARTESIAN_POINT('Ctrl Pts',(29.4683889353564,53.9619749130608,72.904853826243)) ;
#6934 = CARTESIAN_POINT('Ctrl Pts',(29.3619600045789,53.8606102461995,73.0349839991175)) ;
#6935 = CARTESIAN_POINT('Ctrl Pts',(29.7215414387002,53.6935003224137,72.8969989184745)) ;
#6936 = CARTESIAN_POINT('Ctrl Pts',(29.5650860546413,53.6915946088719,72.7784296249195)) ;
#6937 = CARTESIAN_POINT('Ctrl Pts',(29.4614165662687,53.5901950776532,72.9107431890366)) ;
#6938 = CARTESIAN_POINT('Ctrl Pts',(29.9115055718179,53.1525885953454,72.6318830248109)) ;
#6939 = CARTESIAN_POINT('Ctrl Pts',(29.7502308147021,53.1506832357955,72.519960101264)) ;
#6940 = CARTESIAN_POINT('Ctrl Pts',(29.6521604773189,53.0493503316648,72.6565224488048)) ;
#6941 = CARTESIAN_POINT('Ctrl Pts',(30.0022476308534,52.8821999703571,72.4964697871063)) ;
#6942 = CARTESIAN_POINT('Ctrl Pts',(29.8386696042462,52.8802927777291,72.3879401740398)) ;
#6943 = CARTESIAN_POINT('Ctrl Pts',(29.7434802703421,52.7789455602736,72.5265162325635)) ;
#6944 = CARTESIAN_POINT('Ctrl Pts',(30.1752481522115,52.3415574725627,72.2199301771275)) ;
#6945 = CARTESIAN_POINT('Ctrl Pts',(30.0072737051043,52.3396495857223,72.1183311368414)) ;
#6946 = CARTESIAN_POINT('Ctrl Pts',(29.9180030493363,52.238171223764,72.2607032887875)) ;
#6947 = CARTESIAN_POINT('Ctrl Pts',(30.2574477094345,52.0708923183366,72.0788769583042)) ;
#6948 = CARTESIAN_POINT('Ctrl Pts',(30.0873852279632,52.0689860211252,71.9808203864691)) ;
#6949 = CARTESIAN_POINT('Ctrl Pts',(30.0010696677543,51.9676510264301,72.1250989973514)) ;
#6950 = CARTESIAN_POINT('Ctrl Pts',(30.4128652817387,51.5294526417347,71.7918342379605)) ;
#6951 = CARTESIAN_POINT('Ctrl Pts',(30.2388484777668,51.5275461441316,71.7009779039191)) ;
#6952 = CARTESIAN_POINT('Ctrl Pts',(30.1586558523266,51.4261734609838,71.8487228977031)) ;
#6953 = CARTESIAN_POINT('Ctrl Pts',(30.4862356409264,51.2584285629312,71.6455299256122)) ;
#6954 = CARTESIAN_POINT('Ctrl Pts',(30.3103502329215,51.2565228089169,71.5583449567437)) ;
#6955 = CARTESIAN_POINT('Ctrl Pts',(30.2332792416858,51.1551340723184,71.7077317483349)) ;
#6956 = CARTESIAN_POINT('Ctrl Pts',(30.623370841369,50.7168256230282,71.349178490017)) ;
#6957 = CARTESIAN_POINT('Ctrl Pts',(30.4439912380647,50.7149201642829,71.2694333365719)) ;
#6958 = CARTESIAN_POINT('Ctrl Pts',(30.3732265233668,50.613586979054,71.4219436569748)) ;
#6959 = CARTESIAN_POINT('Ctrl Pts',(30.6871919121486,50.4462620313546,71.1990637682367)) ;
#6960 = CARTESIAN_POINT('Ctrl Pts',(30.5061840531774,50.4443547062135,71.1230856787473)) ;
#6961 = CARTESIAN_POINT('Ctrl Pts',(30.4386300692504,50.343001553274,71.2770326034523)) ;
#6962 = CARTESIAN_POINT('Ctrl Pts',(30.8053663173622,49.9056099882931,70.8949668202972)) ;
#6963 = CARTESIAN_POINT('Ctrl Pts',(30.6213369332285,49.9037019096529,70.8266210208818)) ;
#6964 = CARTESIAN_POINT('Ctrl Pts',(30.5603112897766,49.8022062837453,70.9831829221991)) ;
#6965 = CARTESIAN_POINT('Ctrl Pts',(30.8596553784308,49.635040821774,70.7411227832435)) ;
#6966 = CARTESIAN_POINT('Ctrl Pts',(30.6742396913967,49.6331344367333,70.6766456166729)) ;
#6967 = CARTESIAN_POINT('Ctrl Pts',(30.6164673707908,49.5318014383246,70.8345361175774)) ;
#6968 = CARTESIAN_POINT('Ctrl Pts',(30.9584720415982,49.0942250306884,70.4304004819357)) ;
#6969 = CARTESIAN_POINT('Ctrl Pts',(30.7705226537011,49.0923183862279,70.3737276915643)) ;
#6970 = CARTESIAN_POINT('Ctrl Pts',(30.7194087768269,48.9909365753838,70.5338683441997)) ;
#6971 = CARTESIAN_POINT('Ctrl Pts',(31.0030604905696,48.8238179925337,70.2733051326608)) ;
#6972 = CARTESIAN_POINT('Ctrl Pts',(30.8139656641572,48.8219121926088,70.2205800897392)) ;
#6973 = CARTESIAN_POINT('Ctrl Pts',(30.7662145198663,48.720533172951,70.3817571390707)) ;
#6974 = CARTESIAN_POINT('Ctrl Pts',(31.0822781893569,48.2823982253176,69.9566492356375)) ;
#6975 = CARTESIAN_POINT('Ctrl Pts',(30.8911438797355,48.2804926625113,69.9118831048759)) ;
#6976 = CARTESIAN_POINT('Ctrl Pts',(30.8501713843621,48.1791582421951,70.0749415328362)) ;
#6977 = CARTESIAN_POINT('Ctrl Pts',(31.1169423489645,48.0114576298754,69.7969790787265)) ;
#6978 = CARTESIAN_POINT('Ctrl Pts',(30.9249086717214,48.009552069648,69.756223244743)) ;
#6979 = CARTESIAN_POINT('Ctrl Pts',(30.8873821347699,47.9080609643586,69.9200170457096)) ;
#6980 = CARTESIAN_POINT('Ctrl Pts',(31.1762008520855,47.4697670851897,69.475538363929)) ;
#6981 = CARTESIAN_POINT('Ctrl Pts',(30.9826313664683,47.4678622558982,69.4428669398108)) ;
#6982 = CARTESIAN_POINT('Ctrl Pts',(30.9519839904029,47.3665093096401,69.6081666509721)) ;
#6983 = CARTESIAN_POINT('Ctrl Pts',(31.2007210276185,47.1991192501307,69.3142255810316)) ;
#6984 = CARTESIAN_POINT('Ctrl Pts',(31.0065113086846,47.1972127705462,69.2856097758525)) ;
#6985 = CARTESIAN_POINT('Ctrl Pts',(30.9793273889069,47.0958808569866,69.4515263244446)) ;
#6986 = CARTESIAN_POINT('Ctrl Pts',(31.2396113270229,46.6582159321595,68.9904228772838)) ;
#6987 = CARTESIAN_POINT('Ctrl Pts',(31.0443737081918,46.6563091332066,68.9699494408894)) ;
#6988 = CARTESIAN_POINT('Ctrl Pts',(31.0241543176845,46.5549171221787,69.136823273953)) ;
#6989 = CARTESIAN_POINT('Ctrl Pts',(31.2539830666496,46.3878930438546,68.82781193536)) ;
#6990 = CARTESIAN_POINT('Ctrl Pts',(31.0583602495382,46.3859871917592,68.8114299191662)) ;
#6991 = CARTESIAN_POINT('Ctrl Pts',(31.0416355352769,46.2846172014713,68.9787027814551)) ;
#6992 = CARTESIAN_POINT('Ctrl Pts',(31.2724899758963,45.847008993619,68.5022603903092)) ;
#6993 = CARTESIAN_POINT('Ctrl Pts',(31.0763542296701,45.8451033188908,68.4940696998761)) ;
#6994 = CARTESIAN_POINT('Ctrl Pts',(31.0666340319201,45.7437666877133,68.6619144618478)) ;
#6995 = CARTESIAN_POINT('Ctrl Pts',(31.276642725521,45.576594876658,68.3392191581406)) ;
#6996 = CARTESIAN_POINT('Ctrl Pts',(31.0803756867806,45.5746876691305,68.335128608911)) ;
#6997 = CARTESIAN_POINT('Ctrl Pts',(31.0741702161106,45.4732994150359,68.5031114092514)) ;
#6998 = CARTESIAN_POINT('Ctrl Pts',(31.2756697210528,45.3060601767044,68.1759683239932)) ;
#6999 = CARTESIAN_POINT('Ctrl Pts',(31.079403573458,45.3041537286489,68.1759873411111)) ;
#7000 = CARTESIAN_POINT('Ctrl Pts',(31.0767156357415,45.2027271666488,68.3440035995781)) ;
#7001 = CARTESIAN_POINT('Ctrl Pts',(31.2707596705055,45.1993067880441,68.0115966179513)) ;
#7002 = CARTESIAN_POINT('Ctrl Pts',(31.0767059192039,45.2022941676425,68.0161583317382)) ;
#7003 = CARTESIAN_POINT('Ctrl Pts',(31.0685647903147,45.3026134137914,67.8501572385602)) ;
#7004 = CARTESIAN_POINT('Ctrl Pts',(31.2753738913076,45.4820412744326,68.1821045031859)) ;
#7005 = CARTESIAN_POINT('Ctrl Pts',(31.0812188154374,45.485027067948,68.1824209119147)) ;
#7006 = CARTESIAN_POINT('Ctrl Pts',(31.0767098704522,45.5853439255345,68.0162388993778)) ;
#7007 = CARTESIAN_POINT('Ctrl Pts',(31.2743767150006,45.7643410734729,68.3523909127677)) ;
#7008 = CARTESIAN_POINT('Ctrl Pts',(31.0802656447196,45.7673274764098,68.3484647485212)) ;
#7009 = CARTESIAN_POINT('Ctrl Pts',(31.0793851694405,45.8675609241944,68.182178381083)) ;
#7010 = CARTESIAN_POINT('Ctrl Pts',(31.2613182473705,46.3280183066973,68.6918476698476)) ;
#7011 = CARTESIAN_POINT('Ctrl Pts',(31.0675617987265,46.3310049156009,68.6794713223723)) ;
#7012 = CARTESIAN_POINT('Ctrl Pts',(31.0739245141333,46.4312549192508,68.5133137341179)) ;
#7013 = CARTESIAN_POINT('Ctrl Pts',(31.2492433795396,46.6093355962432,68.8612448090648)) ;
#7014 = CARTESIAN_POINT('Ctrl Pts',(31.0558010086264,46.6123217179656,68.844652477278)) ;
#7015 = CARTESIAN_POINT('Ctrl Pts',(31.0657791914954,46.7126174787595,68.6786988015514)) ;
#7016 = CARTESIAN_POINT('Ctrl Pts',(31.2141263134973,47.1717937444718,69.1984722106304)) ;
#7017 = CARTESIAN_POINT('Ctrl Pts',(31.0215907151539,47.1747789756108,69.1734846605815)) ;
#7018 = CARTESIAN_POINT('Ctrl Pts',(31.0387767823933,47.2750030883528,69.0080813459652)) ;
#7019 = CARTESIAN_POINT('Ctrl Pts',(31.1911024008108,47.4527838882087,69.3662496718402)) ;
#7020 = CARTESIAN_POINT('Ctrl Pts',(30.9991541250229,47.4557718391023,69.3370888215369)) ;
#7021 = CARTESIAN_POINT('Ctrl Pts',(31.019928636683,47.5560106521893,69.1721061379612)) ;
#7022 = CARTESIAN_POINT('Ctrl Pts',(31.1341568670205,48.0142871287658,69.7001372321145)) ;
#7023 = CARTESIAN_POINT('Ctrl Pts',(30.9436506057594,48.0172768213744,69.6626716706322)) ;
#7024 = CARTESIAN_POINT('Ctrl Pts',(30.9715585882536,48.1176560532481,69.4988251729331)) ;
#7025 = CARTESIAN_POINT('Ctrl Pts',(31.1002449637116,48.295266819104,69.8661099004534)) ;
#7026 = CARTESIAN_POINT('Ctrl Pts',(30.910603800394,48.2982535237946,69.8245104998946)) ;
#7027 = CARTESIAN_POINT('Ctrl Pts',(30.942078500755,48.3984774868501,69.6612225081025)) ;
#7028 = CARTESIAN_POINT('Ctrl Pts',(31.0217140098796,48.8569739450444,70.1954351770645)) ;
#7029 = CARTESIAN_POINT('Ctrl Pts',(30.8340552348197,48.8599612930095,70.1456443070115)) ;
#7030 = CARTESIAN_POINT('Ctrl Pts',(30.872582034942,48.9602369846067,69.9839049650751)) ;
#7031 = CARTESIAN_POINT('Ctrl Pts',(30.9770284257322,49.1378578224526,70.3590251080683)) ;
#7032 = CARTESIAN_POINT('Ctrl Pts',(30.7904973368589,49.1408439739939,70.3051641970359)) ;
#7033 = CARTESIAN_POINT('Ctrl Pts',(30.8325331930582,49.2411084827197,70.1442945851104)) ;
#7034 = CARTESIAN_POINT('Ctrl Pts',(30.8770845405165,49.7002903800716,70.6829312861811)) ;
#7035 = CARTESIAN_POINT('Ctrl Pts',(30.6930720380202,49.7032760750572,70.6210138296207)) ;
#7036 = CARTESIAN_POINT('Ctrl Pts',(30.742065302515,49.8035038746341,70.4621032079514)) ;
#7037 = CARTESIAN_POINT('Ctrl Pts',(30.8218159490199,49.9815741041477,70.8433329295991)) ;
#7038 = CARTESIAN_POINT('Ctrl Pts',(30.6391884935956,49.9845603797238,70.7774284628369)) ;
#7039 = CARTESIAN_POINT('Ctrl Pts',(30.6916049557576,50.084920629536,70.6196923965754)) ;
#7040 = CARTESIAN_POINT('Ctrl Pts',(30.7005980268366,50.5452598054567,71.1609464797428)) ;
#7041 = CARTESIAN_POINT('Ctrl Pts',(30.5210220118427,50.5482445256766,71.0871424982923)) ;
#7042 = CARTESIAN_POINT('Ctrl Pts',(30.5802875368357,50.6484794514056,70.9317743843129)) ;
#7043 = CARTESIAN_POINT('Ctrl Pts',(30.6347845222986,50.8275371605558,71.3178190881531)) ;
#7044 = CARTESIAN_POINT('Ctrl Pts',(30.4568608995758,50.8305243023805,71.2401164427609)) ;
#7045 = CARTESIAN_POINT('Ctrl Pts',(30.5195054534064,50.9307473367164,71.0860721504808)) ;
#7046 = CARTESIAN_POINT('Ctrl Pts',(30.5281930551463,51.2516112326399,71.5502037790437)) ;
#7047 = CARTESIAN_POINT('Ctrl Pts',(30.3529412567396,51.2545984104442,71.4667251371801)) ;
#7048 = CARTESIAN_POINT('Ctrl Pts',(30.4205752839267,51.3548887142843,71.3148795074004)) ;
#7049 = CARTESIAN_POINT('Ctrl Pts',(30.4913107555821,51.3931523912117,71.6272529315444)) ;
#7050 = CARTESIAN_POINT('Ctrl Pts',(30.3169834983725,51.3961391935532,71.5418590470166)) ;
#7051 = CARTESIAN_POINT('Ctrl Pts',(30.3862730556347,51.4964465474926,71.3907722579837)) ;
#7052 = CARTESIAN_POINT('Ctrl Pts',(30.4151092402135,51.6761627264651,71.7799422493361)) ;
#7053 = CARTESIAN_POINT('Ctrl Pts',(30.242695078949,51.6791488679195,71.6907527013559)) ;
#7054 = CARTESIAN_POINT('Ctrl Pts',(30.3152873232083,51.7794030062388,71.5411913280897)) ;
#7055 = CARTESIAN_POINT('Ctrl Pts',(30.3757935636177,51.8176028378213,71.8555858876626)) ;
#7056 = CARTESIAN_POINT('Ctrl Pts',(30.2043654786474,51.8205891355611,71.7645164524545)) ;
#7057 = CARTESIAN_POINT('Ctrl Pts',(30.2785921329714,51.9208298261689,71.6157510097026)) ;
#7058 = CARTESIAN_POINT('Ctrl Pts',(30.2542175154657,52.2417288193145,72.0804228994921)) ;
#7059 = CARTESIAN_POINT('Ctrl Pts',(30.0858363153209,52.2447151365677,71.9837662267925)) ;
#7060 = CARTESIAN_POINT('Ctrl Pts',(30.1649131134242,52.3449566194198,71.8374878351155)) ;
#7061 = CARTESIAN_POINT('Ctrl Pts',(30.1682702114188,52.5241300049717,72.22762270877)) ;
#7062 = CARTESIAN_POINT('Ctrl Pts',(30.00203922285,52.5271161388606,72.1273087609404)) ;
#7063 = CARTESIAN_POINT('Ctrl Pts',(30.0842751721127,52.6274277787848,71.9828283867849)) ;
#7064 = CARTESIAN_POINT('Ctrl Pts',(29.9869590883597,53.0891744812326,72.5160091947715)) ;
#7065 = CARTESIAN_POINT('Ctrl Pts',(29.8252717919771,53.0921595377507,72.4085302103788)) ;
#7066 = CARTESIAN_POINT('Ctrl Pts',(29.9137644892835,53.1923844744817,72.267737360374)) ;
#7067 = CARTESIAN_POINT('Ctrl Pts',(29.8916728500753,53.371665470285,72.6570941471294)) ;
#7068 = CARTESIAN_POINT('Ctrl Pts',(29.7323692115319,53.3746531996403,72.5461122770274)) ;
#7069 = CARTESIAN_POINT('Ctrl Pts',(29.8239134874277,53.4748857690477,72.4072892427669)) ;
#7070 = CARTESIAN_POINT('Ctrl Pts',(29.6918335619832,53.9365848433157,72.9330442939948)) ;
#7071 = CARTESIAN_POINT('Ctrl Pts',(29.5375242163636,53.9395741566825,72.8152101149305)) ;
#7072 = CARTESIAN_POINT('Ctrl Pts',(29.6350044013411,54.0399343658719,72.6805777758222)) ;
#7073 = CARTESIAN_POINT('Ctrl Pts',(29.5873107371871,54.2194050938079,73.067842310348)) ;
#7074 = CARTESIAN_POINT('Ctrl Pts',(29.4356221911967,54.2223916876785,72.9466599778714)) ;
#7075 = CARTESIAN_POINT('Ctrl Pts',(29.5360678154317,54.3226177650003,72.8141303651837)) ;
#7076 = CARTESIAN_POINT('Ctrl Pts',(29.3695790835415,54.7853172886214,73.3303792062082)) ;
#7077 = CARTESIAN_POINT('Ctrl Pts',(29.2233330805696,54.7883043794011,73.2026795844699)) ;
#7078 = CARTESIAN_POINT('Ctrl Pts',(29.329464103686,54.888570414198,73.0746868570139)) ;
#7079 = CARTESIAN_POINT('Ctrl Pts',(29.2562377433629,55.0683374452758,73.4582537530578)) ;
#7080 = CARTESIAN_POINT('Ctrl Pts',(29.1128251734266,55.0713235720022,73.3273798129575)) ;
#7081 = CARTESIAN_POINT('Ctrl Pts',(29.221732199964,55.1715968138862,73.2017461799581)) ;
#7082 = CARTESIAN_POINT('Ctrl Pts',(29.0219184628403,55.6338317485941,73.7057667733599)) ;
#7083 = CARTESIAN_POINT('Ctrl Pts',(28.884364077656,55.6368172834005,73.5687509636409)) ;
#7084 = CARTESIAN_POINT('Ctrl Pts',(28.9986751021317,55.7370429277092,73.4479765402196)) ;
#7085 = CARTESIAN_POINT('Ctrl Pts',(28.9008692462189,55.9162154787378,73.8255204414319)) ;
#7086 = CARTESIAN_POINT('Ctrl Pts',(28.7663331269695,55.9192018042793,73.6855329720701)) ;
#7087 = CARTESIAN_POINT('Ctrl Pts',(28.8831959257244,56.0195762764982,73.5673440006423)) ;
#7088 = CARTESIAN_POINT('Ctrl Pts',(28.6508660111268,56.4812254904529,74.0571282289314)) ;
#7089 = CARTESIAN_POINT('Ctrl Pts',(28.5225811568725,56.484210134814,73.9113965902898)) ;
#7090 = CARTESIAN_POINT('Ctrl Pts',(28.6445514045126,56.5844490941092,73.798373497653)) ;
#7091 = CARTESIAN_POINT('Ctrl Pts',(28.522236149594,56.7637439358821,74.1686873940088)) ;
#7092 = CARTESIAN_POINT('Ctrl Pts',(28.3971633157449,56.7667309512438,74.0201907033106)) ;
#7093 = CARTESIAN_POINT('Ctrl Pts',(28.5215800577612,56.8669533046419,73.9098522901186)) ;
#7094 = CARTESIAN_POINT('Ctrl Pts',(28.2577296814636,57.3288079962307,74.38332865809)) ;
#7095 = CARTESIAN_POINT('Ctrl Pts',(28.1392580206003,57.3317959921775,74.2295107078863)) ;
#7096 = CARTESIAN_POINT('Ctrl Pts',(28.2683410236814,57.4320972449965,74.1247401072848)) ;
#7097 = CARTESIAN_POINT('Ctrl Pts',(28.1217698050726,57.611503670377,74.4864574136107)) ;
#7098 = CARTESIAN_POINT('Ctrl Pts',(28.0066954436726,57.614489922013,74.3300837580924)) ;
#7099 = CARTESIAN_POINT('Ctrl Pts',(28.1380642361742,57.71473561364,74.2281426830806)) ;
#7100 = CARTESIAN_POINT('Ctrl Pts',(27.843365296793,58.1775332619195,74.6835750662936)) ;
#7101 = CARTESIAN_POINT('Ctrl Pts',(27.735240524604,58.1805194049571,74.5223182830966)) ;
#7102 = CARTESIAN_POINT('Ctrl Pts',(27.8709460181227,58.2807563670581,74.4262173072657)) ;
#7103 = CARTESIAN_POINT('Ctrl Pts',(27.7007840548285,58.4605262973727,74.7776533339454)) ;
#7104 = CARTESIAN_POINT('Ctrl Pts',(27.5962147138393,58.4635110441087,74.614065002193)) ;
#7105 = CARTESIAN_POINT('Ctrl Pts',(27.7339403582833,58.5638587343234,74.5209942372437)) ;
#7106 = CARTESIAN_POINT('Ctrl Pts',(27.5556022785721,58.7433256931628,74.8667534769041)) ;
#7107 = CARTESIAN_POINT('Ctrl Pts',(27.4546609736715,58.7463119239391,74.7009621614397)) ;
#7108 = CARTESIAN_POINT('Ctrl Pts',(27.5944222023064,58.846513767945,74.6108998812056)) ;
#7109 = CARTESIAN_POINT('Origin',(34.2457299930682,45.3830586252741,34.9200048199517)) ;
#7110 = CARTESIAN_POINT('',(25.8874358604319,45.3830610445957,60.805979493395)) ;
#7111 = CARTESIAN_POINT('',(32.227700990655,45.3830586252741,41.2926628570961)) ;
#7112 = CARTESIAN_POINT('',(25.887439674075,45.3830586252741,60.8059807325238)) ;
#7113 = CARTESIAN_POINT('Ctrl Pts',(25.8874344722073,45.3830586252741,60.805979042333)) ;
#7114 = CARTESIAN_POINT('Ctrl Pts',(25.8831617902991,45.3830586252741,60.8191290015772)) ;
#7115 = CARTESIAN_POINT('Ctrl Pts',(25.8805089846612,45.3830586252741,60.8327110288752)) ;
#7116 = CARTESIAN_POINT('Ctrl Pts',(25.8783596228545,45.3830586252741,60.861390991021)) ;
#7117 = CARTESIAN_POINT('Ctrl Pts',(25.8791455812147,45.3830586252741,60.876331277846)) ;
#7118 = CARTESIAN_POINT('Ctrl Pts',(25.8863194956573,45.3830586252741,60.9178099819017)) ;
#7119 = CARTESIAN_POINT('Ctrl Pts',(25.8966456738107,45.3830586252741,60.9432469495347)) ;
#7120 = CARTESIAN_POINT('Ctrl Pts',(25.9270686569879,45.3830586252741,60.9910540894173)) ;
#7121 = CARTESIAN_POINT('Ctrl Pts',(25.9476816529992,45.3830586252736,61.0126928579513)) ;
#7122 = CARTESIAN_POINT('Ctrl Pts',(25.9926879310718,45.3830586252736,61.0462961404911)) ;
#7123 = CARTESIAN_POINT('Ctrl Pts',(26.0164911651481,45.3830586252741,61.0589713793357)) ;
#7124 = CARTESIAN_POINT('Ctrl Pts',(26.0416005791977,45.3830586252741,61.0679696745342)) ;
#7125 = CARTESIAN_POINT('',(25.7914429954097,45.3830674541108,60.7777739865218)) ;
#7126 = CARTESIAN_POINT('Ctrl Pts',(25.5149631682037,45.3830586252741,60.9005821812565)) ;
#7127 = CARTESIAN_POINT('Ctrl Pts',(25.540242497525,45.3830586252741,60.9076155911763)) ;
#7128 = CARTESIAN_POINT('Ctrl Pts',(25.5665430671899,45.3830586252745,60.9110143156868)) ;
#7129 = CARTESIAN_POINT('Ctrl Pts',(25.6223302267837,45.3830586252745,60.9098503269198)) ;
#7130 = CARTESIAN_POINT('Ctrl Pts',(25.651747876875,45.3830586252741,60.9042145461539)) ;
#7131 = CARTESIAN_POINT('Ctrl Pts',(25.7044084924816,45.3830586252741,60.8829582286584)) ;
#7132 = CARTESIAN_POINT('Ctrl Pts',(25.7276504263598,45.3830586252741,60.8682338698508)) ;
#7133 = CARTESIAN_POINT('Ctrl Pts',(25.7574812296411,45.3830586252741,60.8387754420949)) ;
#7134 = CARTESIAN_POINT('Ctrl Pts',(25.7666879461075,45.3830586252741,60.8272731403928)) ;
#7135 = CARTESIAN_POINT('Ctrl Pts',(25.7814944876552,45.3830586252741,60.8031132388058)) ;
#7136 = CARTESIAN_POINT('Ctrl Pts',(25.787226289558,45.3830586252741,60.7907346901948)) ;
#7137 = CARTESIAN_POINT('Ctrl Pts',(25.7914379104393,45.3830586252741,60.7777724061309)) ;
#7138 = CARTESIAN_POINT('',(31.768269675766,45.3830586252741,42.3830402536426)) ;
#7139 = CARTESIAN_POINT('',(31.768269675766,45.3830586252741,42.3830402536426)) ;
#7140 = CARTESIAN_POINT('Origin',(38.4256652898321,45.3830586252741,44.5461592142672)) ;
#7141 = CARTESIAN_POINT('Ctrl Pts',(25.7953108450845,45.383050240221,61.0895083639021)) ;
#7142 = CARTESIAN_POINT('Ctrl Pts',(26.1250882066852,45.9804808943743,61.1966592874771)) ;
#7143 = CARTESIAN_POINT('Ctrl Pts',(26.443572067289,46.5779115664506,61.3337813469064)) ;
#7144 = CARTESIAN_POINT('Ctrl Pts',(26.7620536881248,47.1753380370388,61.4709024420119)) ;
#7145 = CARTESIAN_POINT('Ctrl Pts',(27.0665247840196,47.772764507627,61.6368243793731)) ;
#7146 = CARTESIAN_POINT('Ctrl Pts',(27.3709958799144,48.3701909782152,61.8027463167343)) ;
#7147 = CARTESIAN_POINT('Ctrl Pts',(27.6588588108316,48.9676174488035,61.9960535088842)) ;
#7148 = CARTESIAN_POINT('Ctrl Pts',(27.9467217417488,49.5650439193917,62.1893607010341)) ;
#7149 = CARTESIAN_POINT('Ctrl Pts',(28.2155205626593,50.16247038998,62.4084039191674)) ;
#7150 = CARTESIAN_POINT('Ctrl Pts',(28.4843193835699,50.7598968605682,62.6274471373006)) ;
#7151 = CARTESIAN_POINT('Ctrl Pts',(28.7317607977096,51.3573233311564,62.8703575819127)) ;
#7152 = CARTESIAN_POINT('Ctrl Pts',(28.9792022118494,51.9547498017447,63.1132680265248)) ;
#7153 = CARTESIAN_POINT('Ctrl Pts',(29.2031751363182,52.5521762723329,63.3779732713499)) ;
#7154 = CARTESIAN_POINT('Ctrl Pts',(29.4271480607871,53.1496027429211,63.6426785161751)) ;
#7155 = CARTESIAN_POINT('Ctrl Pts',(29.6257416375641,53.7470292135094,63.9269201893971)) ;
#7156 = CARTESIAN_POINT('Ctrl Pts',(29.8243352143411,54.3444556840976,64.211161862619)) ;
#7157 = CARTESIAN_POINT('Ctrl Pts',(29.9958551130514,54.9418821546858,64.5125149145025)) ;
#7158 = CARTESIAN_POINT('Ctrl Pts',(30.1673750117617,55.5393086252741,64.813867966386)) ;
#7159 = CARTESIAN_POINT('Ctrl Pts',(30.3103578851056,56.1367350958623,65.1297613589466)) ;
#7160 = CARTESIAN_POINT('Ctrl Pts',(30.4533407584495,56.7341615664506,65.4456547515071)) ;
#7161 = CARTESIAN_POINT('Ctrl Pts',(30.5665667269661,57.3315880370388,65.7733933937002)) ;
#7162 = CARTESIAN_POINT('Ctrl Pts',(30.6661847295087,57.8572133193466,66.0617430481042)) ;
#7163 = CARTESIAN_POINT('Ctrl Pts',(30.7420543581155,58.3830758086166,66.3572308973985)) ;
#7164 = CARTESIAN_POINT('Ctrl Pts',(34.2932612192744,45.383050240221,34.9354486515399)) ;
#7165 = CARTESIAN_POINT('Ctrl Pts',(35.8322222400776,45.9804808943743,35.4354862948897)) ;
#7166 = CARTESIAN_POINT('Ctrl Pts',(37.3184802562288,46.5779115664506,36.0753892388935)) ;
#7167 = CARTESIAN_POINT('Ctrl Pts',(38.804727820129,47.1753380370388,36.7152876827189)) ;
#7168 = CARTESIAN_POINT('Ctrl Pts',(40.2255929343049,47.772764507627,37.4895900570713)) ;
#7169 = CARTESIAN_POINT('Ctrl Pts',(41.6464580484807,48.3701909782152,38.2638924314238)) ;
#7170 = CARTESIAN_POINT('Ctrl Pts',(42.9898183927608,48.9676174488035,39.1659926614565)) ;
#7171 = CARTESIAN_POINT('Ctrl Pts',(44.333178737041,49.5650439193917,40.0680928914892)) ;
#7172 = CARTESIAN_POINT('Ctrl Pts',(45.5875732346236,50.16247038998,41.0902945761112)) ;
#7173 = CARTESIAN_POINT('Ctrl Pts',(46.8419677322063,50.7598968605682,42.1124962607332)) ;
#7174 = CARTESIAN_POINT('Ctrl Pts',(47.996694331525,51.3573233311564,43.2460783355894)) ;
#7175 = CARTESIAN_POINT('Ctrl Pts',(49.1514209308438,51.9547498017447,44.3796604104456)) ;
#7176 = CARTESIAN_POINT('Ctrl Pts',(50.1966279116985,52.5521762723329,45.6149515529632)) ;
#7177 = CARTESIAN_POINT('Ctrl Pts',(51.2418348925531,53.1496027429211,46.8502426954807)) ;
#7178 = CARTESIAN_POINT('Ctrl Pts',(52.1686049175126,53.7470292135094,48.176703837183)) ;
#7179 = CARTESIAN_POINT('Ctrl Pts',(53.0953749424721,54.3444556840976,49.5031649788854)) ;
#7180 = CARTESIAN_POINT('Ctrl Pts',(53.8958011364534,54.9418821546858,50.9094792210085)) ;
#7181 = CARTESIAN_POINT('Ctrl Pts',(54.6962273304346,55.5393086252741,52.3157934631316)) ;
#7182 = CARTESIAN_POINT('Ctrl Pts',(55.363480739373,56.1367350958623,53.7899626284141)) ;
#7183 = CARTESIAN_POINT('Ctrl Pts',(56.0307341483113,56.7341615664505,55.2641317936966)) ;
#7184 = CARTESIAN_POINT('Ctrl Pts',(56.5591220013886,57.3315880370388,56.7935787905978)) ;
#7185 = CARTESIAN_POINT('Ctrl Pts',(57.0240060132542,57.8572133193466,58.1392105111498)) ;
#7186 = CARTESIAN_POINT('Ctrl Pts',(57.3780642800859,58.3830758086166,59.5181538078565)) ;
#7187 = CARTESIAN_POINT('',(49.6868966603788,58.3353824278239,61.3897862372794)) ;
#7188 = CARTESIAN_POINT('',(31.0053184302396,58.2172712656978,66.1863974475356)) ;
#7189 = CARTESIAN_POINT('Ctrl Pts',(49.6868966603788,58.3353824278239,61.3897862372794)) ;
#7190 = CARTESIAN_POINT('Ctrl Pts',(47.1887437966009,58.3308357090662,62.0312028752173)) ;
#7191 = CARTESIAN_POINT('Ctrl Pts',(44.3889324086846,58.3244410141137,62.7500722580065)) ;
#7192 = CARTESIAN_POINT('Ctrl Pts',(39.5787343864927,58.306635184046,63.9851211967428)) ;
#7193 = CARTESIAN_POINT('Ctrl Pts',(34.295419682726,58.2895264446021,65.3416458528576)) ;
#7194 = CARTESIAN_POINT('Ctrl Pts',(31.0053191458883,58.2172696107889,66.1864000932465)) ;
#7195 = CARTESIAN_POINT('Ctrl Pts',(31.0053184302396,58.2172712656978,66.1863974475356)) ;
#7196 = CARTESIAN_POINT('Ctrl Pts',(30.9631600045902,57.9495340002377,66.0305344100695)) ;
#7197 = CARTESIAN_POINT('Ctrl Pts',(30.916172209291,57.6819084045908,65.8760449063787)) ;
#7198 = CARTESIAN_POINT('Ctrl Pts',(30.8645011127033,57.4145313636581,65.7233157164034)) ;
#7199 = CARTESIAN_POINT('Ctrl Pts',(30.816535099193,57.1663266301673,65.5815379939713)) ;
#7200 = CARTESIAN_POINT('Ctrl Pts',(30.7645218642245,56.9182638872656,65.4412351217362)) ;
#7201 = CARTESIAN_POINT('Ctrl Pts',(30.7085361013266,56.6702295478714,65.3025887342681)) ;
#7202 = CARTESIAN_POINT('Ctrl Pts',(30.7042115413412,56.6510704023381,65.2918791433234)) ;
#7203 = CARTESIAN_POINT('Ctrl Pts',(30.6998629795545,56.6319118940957,65.2811786693435)) ;
#7204 = CARTESIAN_POINT('Ctrl Pts',(30.6954904598184,56.612753845668,65.2704874240641)) ;
#7205 = CARTESIAN_POINT('Ctrl Pts',(30.6381436909714,56.3614909032359,65.1302688753267)) ;
#7206 = CARTESIAN_POINT('Ctrl Pts',(30.576681027564,56.1103350670457,64.9916539487321)) ;
#7207 = CARTESIAN_POINT('Ctrl Pts',(30.5112384716708,55.8590202585562,64.8549672058044)) ;
#7208 = CARTESIAN_POINT('Ctrl Pts',(30.5070932757221,55.8431017310512,64.8463093328762)) ;
#7209 = CARTESIAN_POINT('Ctrl Pts',(30.5029322656911,55.8271830724927,64.8376594291815)) ;
#7210 = CARTESIAN_POINT('Ctrl Pts',(30.4987554443582,55.8112643008985,64.8290175054764)) ;
#7211 = CARTESIAN_POINT('Ctrl Pts',(30.4319637016308,55.5567064895581,64.6908241046145)) ;
#7212 = CARTESIAN_POINT('Ctrl Pts',(30.3610954434403,55.3019957844227,64.5546044340852)) ;
#7213 = CARTESIAN_POINT('Ctrl Pts',(30.286151897374,55.0471908391173,64.420397343297)) ;
#7214 = CARTESIAN_POINT('Ctrl Pts',(30.2824189305709,55.0344989069627,64.4137124365778)) ;
#7215 = CARTESIAN_POINT('Ctrl Pts',(30.2786758239704,55.0218058655742,64.4070325703337)) ;
#7216 = CARTESIAN_POINT('Ctrl Pts',(30.2749226306752,55.0091118266697,64.4003578297875)) ;
#7217 = CARTESIAN_POINT('Ctrl Pts',(30.1986055999066,54.7509925981972,64.2646343699017)) ;
#7218 = CARTESIAN_POINT('Ctrl Pts',(30.1181614779075,54.4926055131012,64.1311058189801)) ;
#7219 = CARTESIAN_POINT('Ctrl Pts',(30.0339415706751,54.2345762733045,64.0003253705781)) ;
#7220 = CARTESIAN_POINT('Ctrl Pts',(30.030867315893,54.2251575070005,63.9955515299017)) ;
#7221 = CARTESIAN_POINT('Ctrl Pts',(30.027787792249,54.2157389752755,63.9907809698703)) ;
#7222 = CARTESIAN_POINT('Ctrl Pts',(30.0247030062888,54.2063206495465,63.9860136998315)) ;
#7223 = CARTESIAN_POINT('Ctrl Pts',(29.9391306767364,53.9450551732693,63.8537690617642)) ;
#7224 = CARTESIAN_POINT('Ctrl Pts',(29.8495437893631,53.6840579939692,63.7241124455533)) ;
#7225 = CARTESIAN_POINT('Ctrl Pts',(29.7562013732715,53.4230444575823,63.5974004437296)) ;
#7226 = CARTESIAN_POINT('Ctrl Pts',(29.7539970080238,53.4168803877747,63.5944080256523)) ;
#7227 = CARTESIAN_POINT('Ctrl Pts',(29.7517905621932,53.4107163826998,63.5914172584352)) ;
#7228 = CARTESIAN_POINT('Ctrl Pts',(29.7495820361275,53.4045524432162,63.5884281424623)) ;
#7229 = CARTESIAN_POINT('Ctrl Pts',(29.6548939042669,53.1402803009606,63.4602730747941)) ;
#7230 = CARTESIAN_POINT('Ctrl Pts',(29.5563551294916,52.8760533725781,63.3351165968918)) ;
#7231 = CARTESIAN_POINT('Ctrl Pts',(29.4539651627725,52.6118787196958,63.2129643349594)) ;
#7232 = CARTESIAN_POINT('Ctrl Pts',(29.34932817923,52.3419065760205,63.0881313593168)) ;
#7233 = CARTESIAN_POINT('Ctrl Pts',(29.2407203431504,52.0715787920593,62.966514326652)) ;
#7234 = CARTESIAN_POINT('Ctrl Pts',(29.1283839508344,51.8011908422986,62.8483944694407)) ;
#7235 = CARTESIAN_POINT('Ctrl Pts',(29.1282429199986,51.8008513882913,62.8482461778511)) ;
#7236 = CARTESIAN_POINT('Ctrl Pts',(29.1281018832898,51.8005119341973,62.8480978917768)) ;
#7237 = CARTESIAN_POINT('Ctrl Pts',(29.1279608407085,51.8001724800172,62.8479496112184)) ;
#7238 = CARTESIAN_POINT('Ctrl Pts',(29.0169624142087,51.5330270582816,62.7312550036823)) ;
#7239 = CARTESIAN_POINT('Ctrl Pts',(28.9020807918313,51.265585354454,62.6177412654934)) ;
#7240 = CARTESIAN_POINT('Ctrl Pts',(28.7840333481004,50.998401550286,62.5081218916898)) ;
#7241 = CARTESIAN_POINT('Ctrl Pts',(28.7824465405845,50.9948100344075,62.5066483752736)) ;
#7242 = CARTESIAN_POINT('Ctrl Pts',(28.7808591533881,50.9912185474961,62.5051755551275)) ;
#7243 = CARTESIAN_POINT('Ctrl Pts',(28.7792711881907,50.9876270907846,62.5037034329515)) ;
#7244 = CARTESIAN_POINT('Ctrl Pts',(28.6625754771975,50.723699647587,62.395520744638)) ;
#7245 = CARTESIAN_POINT('Ctrl Pts',(28.5427137344922,50.4599498020535,62.2910367586478)) ;
#7246 = CARTESIAN_POINT('Ctrl Pts',(28.4196910854721,50.1963788513665,62.190246712141)) ;
#7247 = CARTESIAN_POINT('Ctrl Pts',(28.4165103624189,50.1895642834337,62.1876408080492)) ;
#7248 = CARTESIAN_POINT('Ctrl Pts',(28.4133276054837,50.1827500045962,62.1850374381137)) ;
#7249 = CARTESIAN_POINT('Ctrl Pts',(28.4101428122157,50.1759360087369,62.1824365995409)) ;
#7250 = CARTESIAN_POINT('Ctrl Pts',(28.2884713276816,49.9156148757614,62.0830744546357)) ;
#7251 = CARTESIAN_POINT('Ctrl Pts',(28.1639337475715,49.6552611188173,61.9874999665714)) ;
#7252 = CARTESIAN_POINT('Ctrl Pts',(28.036582698318,49.394895725602,61.8957330403494)) ;
#7253 = CARTESIAN_POINT('Ctrl Pts',(28.0316485060048,49.3848079176934,61.8921775481519)) ;
#7254 = CARTESIAN_POINT('Ctrl Pts',(28.0267101929823,49.3747203101762,61.8886278536189)) ;
#7255 = CARTESIAN_POINT('Ctrl Pts',(28.0217677725964,49.3646329259557,61.885083965985)) ;
#7256 = CARTESIAN_POINT('Ctrl Pts',(27.8958077613399,49.1075509841625,61.7947662488741)) ;
#7257 = CARTESIAN_POINT('Ctrl Pts',(27.7670101513391,48.8504690628023,61.7081075507894)) ;
#7258 = CARTESIAN_POINT('Ctrl Pts',(27.6357590860055,48.5931578990173,61.6253810703911)) ;
#7259 = CARTESIAN_POINT('Ctrl Pts',(27.6289499859684,48.579808998188,61.6210893499443)) ;
#7260 = CARTESIAN_POINT('Ctrl Pts',(27.6221340729031,48.5664590689812,61.6168080801546)) ;
#7261 = CARTESIAN_POINT('Ctrl Pts',(27.6153114131665,48.5531081058638,61.6125373090307)) ;
#7262 = CARTESIAN_POINT('Ctrl Pts',(27.4854613464429,48.299010214641,61.5312552376969)) ;
#7263 = CARTESIAN_POINT('Ctrl Pts',(27.3530838160539,48.0446012919298,61.4537190910644)) ;
#7264 = CARTESIAN_POINT('Ctrl Pts',(27.2184975701169,47.7903648312084,61.380137994295)) ;
#7265 = CARTESIAN_POINT('Ctrl Pts',(27.2097182717112,47.7737805380754,61.375338169461)) ;
#7266 = CARTESIAN_POINT('Ctrl Pts',(27.2009292477176,47.7571963611374,61.3705549960484)) ;
#7267 = CARTESIAN_POINT('Ctrl Pts',(27.1921305426904,47.7406123516807,61.3657885082833)) ;
#7268 = CARTESIAN_POINT('Ctrl Pts',(27.0589583567007,47.4896062337362,61.293645665307)) ;
#7269 = CARTESIAN_POINT('Ctrl Pts',(26.9239230943588,47.2387261489803,61.2255064278626)) ;
#7270 = CARTESIAN_POINT('Ctrl Pts',(26.7869892778423,46.9878897404753,61.161330116392)) ;
#7271 = CARTESIAN_POINT('Ctrl Pts',(26.7762121770987,46.9681481652137,61.1562792488147)) ;
#7272 = CARTESIAN_POINT('Ctrl Pts',(26.7654236325356,46.9484074501541,61.1512530906726)) ;
#7273 = CARTESIAN_POINT('Ctrl Pts',(26.7546236456281,46.9286675886394,61.1462516297055)) ;
#7274 = CARTESIAN_POINT('Ctrl Pts',(26.6191325753522,46.6810214584507,61.0835058777729)) ;
#7275 = CARTESIAN_POINT('Ctrl Pts',(26.4817445180494,46.4334531760671,61.0246143969619)) ;
#7276 = CARTESIAN_POINT('Ctrl Pts',(26.3428384963142,46.1857600468481,60.9697398855416)) ;
#7277 = CARTESIAN_POINT('Ctrl Pts',(26.3300701725596,46.1629919477681,60.9646957879644)) ;
#7278 = CARTESIAN_POINT('Ctrl Pts',(26.3172887509827,46.1402223084084,60.9596855249274)) ;
#7279 = CARTESIAN_POINT('Ctrl Pts',(26.304494549103,46.1174510138865,60.9547092356778)) ;
#7280 = CARTESIAN_POINT('Ctrl Pts',(26.1670065692551,45.8727480373512,60.9012334532495)) ;
#7281 = CARTESIAN_POINT('Ctrl Pts',(26.0279686867119,45.6279743432132,60.8516422216231)) ;
#7282 = CARTESIAN_POINT('Ctrl Pts',(25.8874358604319,45.3830610445957,60.805979493395)) ;
#7283 = CARTESIAN_POINT('',(42.1202667432172,48.5844537758935,38.6005793350086)) ;
#7284 = CARTESIAN_POINT('Ctrl Pts',(32.227700990655,45.383058625274,41.2926628570961)) ;
#7285 = CARTESIAN_POINT('Ctrl Pts',(32.4703899720628,45.4231928758841,40.830336338963)) ;
#7286 = CARTESIAN_POINT('Ctrl Pts',(32.7630296802974,45.4870033972977,40.3986149672707)) ;
#7287 = CARTESIAN_POINT('Ctrl Pts',(33.4409454321429,45.6539797372435,39.6033827587367)) ;
#7288 = CARTESIAN_POINT('Ctrl Pts',(33.825622182829,45.7573388893141,39.2441406810169)) ;
#7289 = CARTESIAN_POINT('Ctrl Pts',(34.9795172547242,46.0833507061678,38.384504696658)) ;
#7290 = CARTESIAN_POINT('Ctrl Pts',(35.8090454233237,46.3336877227691,37.9915129106226)) ;
#7291 = CARTESIAN_POINT('Ctrl Pts',(37.6274532001708,46.9107591797132,37.5234367516571)) ;
#7292 = CARTESIAN_POINT('Ctrl Pts',(38.6080420354761,47.2383195349501,37.482360447981)) ;
#7293 = CARTESIAN_POINT('Ctrl Pts',(40.4703782091507,47.9083523080807,37.7881695846108)) ;
#7294 = CARTESIAN_POINT('Ctrl Pts',(41.3401309150115,48.2450338483642,38.1158005542573)) ;
#7295 = CARTESIAN_POINT('Ctrl Pts',(42.1202667432172,48.5844537758935,38.6005793350086)) ;
#7296 = CARTESIAN_POINT('',(42.1626024098661,48.6029307720944,38.627181180176)) ;
#7297 = CARTESIAN_POINT('Origin',(60.4279175216359,48.3752007879039,9.69543902564879)) ;
#7298 = CARTESIAN_POINT('',(54.0630686773494,55.0677871747466,51.2065737916888)) ;
#7299 = CARTESIAN_POINT('Ctrl Pts',(42.1626024098661,48.6029307720944,38.6271811801759)) ;
#7300 = CARTESIAN_POINT('Ctrl Pts',(42.5799907523713,48.785356686239,38.8907831019043)) ;
#7301 = CARTESIAN_POINT('Ctrl Pts',(42.9898183927608,48.9676174488035,39.1659926614565)) ;
#7302 = CARTESIAN_POINT('Ctrl Pts',(44.333178737041,49.5650439193917,40.0680928914892)) ;
#7303 = CARTESIAN_POINT('Ctrl Pts',(45.5875732346236,50.16247038998,41.0902945761112)) ;
#7304 = CARTESIAN_POINT('Ctrl Pts',(46.8419677322063,50.7598968605682,42.1124962607332)) ;
#7305 = CARTESIAN_POINT('Ctrl Pts',(47.996694331525,51.3573233311564,43.2460783355894)) ;
#7306 = CARTESIAN_POINT('Ctrl Pts',(49.1514209308438,51.9547498017447,44.3796604104456)) ;
#7307 = CARTESIAN_POINT('Ctrl Pts',(50.1966279116985,52.5521762723329,45.6149515529632)) ;
#7308 = CARTESIAN_POINT('Ctrl Pts',(51.2418348925531,53.1496027429211,46.8502426954807)) ;
#7309 = CARTESIAN_POINT('Ctrl Pts',(52.1686049175126,53.7470292135094,48.176703837183)) ;
#7310 = CARTESIAN_POINT('Ctrl Pts',(53.0953749424721,54.3444556840976,49.5031649788854)) ;
#7311 = CARTESIAN_POINT('Ctrl Pts',(53.8958011364534,54.9418821546858,50.9094792210085)) ;
#7312 = CARTESIAN_POINT('Ctrl Pts',(53.9801273110062,55.0048219850164,51.0576366665657)) ;
#7313 = CARTESIAN_POINT('Ctrl Pts',(54.0630686773494,55.0677871747466,51.2065737916888)) ;
#7314 = CARTESIAN_POINT('',(54.0872831542006,55.0862551252693,51.2503188022344)) ;
#7315 = CARTESIAN_POINT('Origin',(82.7833587713902,55.5110797216523,35.2300331498311)) ;
#7316 = CARTESIAN_POINT('Ctrl Pts',(54.0872831542006,55.0862551252692,51.2503188022345)) ;
#7317 = CARTESIAN_POINT('Ctrl Pts',(54.3470010643438,55.2861476150251,51.7251031936918)) ;
#7318 = CARTESIAN_POINT('Ctrl Pts',(54.5509877839354,55.4856143511658,52.2287777171693)) ;
#7319 = CARTESIAN_POINT('Ctrl Pts',(54.8490787537451,55.8948726679074,53.3113250710519)) ;
#7320 = CARTESIAN_POINT('Ctrl Pts',(54.9333764062709,56.1030296514257,53.8897438782962)) ;
#7321 = CARTESIAN_POINT('Ctrl Pts',(54.9633976722849,56.6395227887269,55.4316582479349)) ;
#7322 = CARTESIAN_POINT('Ctrl Pts',(54.7851691784216,56.9553075668517,56.3910586193405)) ;
#7323 = CARTESIAN_POINT('Ctrl Pts',(54.0695245392049,57.5027527547765,58.1177679371648)) ;
#7324 = CARTESIAN_POINT('Ctrl Pts',(53.5665957257014,57.7356391827932,58.8811489132992)) ;
#7325 = CARTESIAN_POINT('Ctrl Pts',(52.4516508982578,58.0583686966731,60.0088645791411)) ;
#7326 = CARTESIAN_POINT('Ctrl Pts',(51.9093090058447,58.1679507066731,60.4197637200829)) ;
#7327 = CARTESIAN_POINT('Ctrl Pts',(50.8007524922932,58.3023925205291,61.0277068918718)) ;
#7328 = CARTESIAN_POINT('Ctrl Pts',(50.2547155520565,58.3364158765144,61.2439951250786)) ;
#7329 = CARTESIAN_POINT('Ctrl Pts',(49.6868966603788,58.3353824278239,61.3897862372793)) ;
#7330 = CARTESIAN_POINT('Ctrl Pts',(34.1981770821883,45.3830585852922,34.9045538815956)) ;
#7331 = CARTESIAN_POINT('Ctrl Pts',(35.7385556831727,45.9804850758286,35.4001920200424)) ;
#7332 = CARTESIAN_POINT('Ctrl Pts',(37.2266315807177,46.5779115664506,36.0358440646385)) ;
#7333 = CARTESIAN_POINT('Ctrl Pts',(38.7147074283626,47.1753380370388,36.6714960879191)) ;
#7334 = CARTESIAN_POINT('Ctrl Pts',(40.1377848374042,47.772764507627,37.4417388489498)) ;
#7335 = CARTESIAN_POINT('Ctrl Pts',(41.5608622464458,48.3701909782153,38.2119816099806)) ;
#7336 = CARTESIAN_POINT('Ctrl Pts',(42.9068000221931,48.9676174488035,39.1102436691043)) ;
#7337 = CARTESIAN_POINT('Ctrl Pts',(44.2527377979404,49.5650439193917,40.008505728228)) ;
#7338 = CARTESIAN_POINT('Ctrl Pts',(45.5100528738551,50.16247038998,41.0271234302745)) ;
#7339 = CARTESIAN_POINT('Ctrl Pts',(46.7673679497698,50.7598968605682,42.045741132321)) ;
#7340 = CARTESIAN_POINT('Ctrl Pts',(47.9253333569409,51.3573233311564,43.176023990211)) ;
#7341 = CARTESIAN_POINT('Ctrl Pts',(49.083298764112,51.9547498017447,44.3063068481009)) ;
#7342 = CARTESIAN_POINT('Ctrl Pts',(50.1320351499726,52.5521762723329,45.5386116870173)) ;
#7343 = CARTESIAN_POINT('Ctrl Pts',(51.1807715358333,53.1496027429211,46.7709165259337)) ;
#7344 = CARTESIAN_POINT('Ctrl Pts',(52.1113314513134,53.7470292135094,48.0947297554893)) ;
#7345 = CARTESIAN_POINT('Ctrl Pts',(53.0418913667935,54.3444556840976,49.4185429850449)) ;
#7346 = CARTESIAN_POINT('Ctrl Pts',(53.8463356028003,54.9418821546858,50.8225702975286)) ;
#7347 = CARTESIAN_POINT('Ctrl Pts',(54.6507798388072,55.5393086252741,52.2265976100123)) ;
#7348 = CARTESIAN_POINT('Ctrl Pts',(55.3222451607582,56.1367350958623,53.6988603394401)) ;
#7349 = CARTESIAN_POINT('Ctrl Pts',(55.9937104827092,56.7341615664505,55.1711230688678)) ;
#7350 = CARTESIAN_POINT('Ctrl Pts',(56.5264681852295,57.3315880370388,56.6990603887373)) ;
#7351 = CARTESIAN_POINT('Ctrl Pts',(56.9952159947389,57.857234776835,58.0434187497113)) ;
#7352 = CARTESIAN_POINT('Ctrl Pts',(57.3532241458314,58.3831186720347,59.421407891683)) ;
#7353 = CARTESIAN_POINT('Ctrl Pts',(25.7002097997771,45.3830585852922,61.058608161473)) ;
#7354 = CARTESIAN_POINT('Ctrl Pts',(26.0314134558695,45.9804850758286,61.1613615482693)) ;
#7355 = CARTESIAN_POINT('Ctrl Pts',(26.3517233687144,46.5779115664506,61.2942362262193)) ;
#7356 = CARTESIAN_POINT('Ctrl Pts',(26.6720332708182,47.1753380370388,61.4271108997137)) ;
#7357 = CARTESIAN_POINT('Ctrl Pts',(26.9787166592112,47.772764507627,61.588973222463)) ;
#7358 = CARTESIAN_POINT('Ctrl Pts',(27.2854000476041,48.3701909782152,61.7508355452123)) ;
#7359 = CARTESIAN_POINT('Ctrl Pts',(27.57584040775,48.9676174488035,61.9403045649499)) ;
#7360 = CARTESIAN_POINT('Ctrl Pts',(27.8662807678958,49.5650439193917,62.1297735846875)) ;
#7361 = CARTESIAN_POINT('Ctrl Pts',(28.1380001650482,50.16247038998,62.345232818542)) ;
#7362 = CARTESIAN_POINT('Ctrl Pts',(28.4097195622005,50.7598968605682,62.5606920523965)) ;
#7363 = CARTESIAN_POINT('Ctrl Pts',(28.6603997822684,51.3573233311564,62.8003032781533)) ;
#7364 = CARTESIAN_POINT('Ctrl Pts',(28.9110800023363,51.9547498017447,63.0399145039102)) ;
#7365 = CARTESIAN_POINT('Ctrl Pts',(29.1385823300695,52.5521762723329,63.3016334430758)) ;
#7366 = CARTESIAN_POINT('Ctrl Pts',(29.3660846578027,53.1496027429211,63.5633523822414)) ;
#7367 = CARTESIAN_POINT('Ctrl Pts',(29.568468123556,53.7470292135094,63.8449461411063)) ;
#7368 = CARTESIAN_POINT('Ctrl Pts',(29.7708515893093,54.3444556840976,64.1265398999712)) ;
#7369 = CARTESIAN_POINT('Ctrl Pts',(29.9463895287114,54.9418821546858,64.4256060198719)) ;
#7370 = CARTESIAN_POINT('Ctrl Pts',(30.1219274681135,55.5393086252741,64.7246721397726)) ;
#7371 = CARTESIAN_POINT('Ctrl Pts',(30.2691222533582,56.1367350958623,65.0386590940219)) ;
#7372 = CARTESIAN_POINT('Ctrl Pts',(30.4163170386029,56.7341615664506,65.3526460482712)) ;
#7373 = CARTESIAN_POINT('Ctrl Pts',(30.5339128556821,57.3315880370388,65.6788750108841)) ;
#7374 = CARTESIAN_POINT('Ctrl Pts',(30.6373797439176,57.8572347768351,65.965908142268)) ;
#7375 = CARTESIAN_POINT('Ctrl Pts',(30.7171914921666,58.3831186720347,66.2603966824774)) ;
#7376 = CARTESIAN_POINT('',(31.0031929801423,58.3830537363178,66.1869634870219)) ;
#7377 = CARTESIAN_POINT('Ctrl Pts',(25.7914429954097,45.3830674541108,60.7777739865218)) ;
#7378 = CARTESIAN_POINT('Ctrl Pts',(25.8011520792638,45.3999249614349,60.7807915393391)) ;
#7379 = CARTESIAN_POINT('Ctrl Pts',(25.810991377335,45.4170195560983,60.783870696162)) ;
#7380 = CARTESIAN_POINT('Ctrl Pts',(25.8305174186758,45.4509660823352,60.7900238219679)) ;
#7381 = CARTESIAN_POINT('Ctrl Pts',(25.8402729717326,45.4679374856688,60.793119176787)) ;
#7382 = CARTESIAN_POINT('Ctrl Pts',(25.8695171038289,45.5188462146264,60.8024615163315)) ;
#7383 = CARTESIAN_POINT('Ctrl Pts',(25.8889831559,45.5527780591986,60.8087647757947)) ;
#7384 = CARTESIAN_POINT('Ctrl Pts',(25.9472902038144,45.6545524513439,60.8278988611025)) ;
#7385 = CARTESIAN_POINT('Ctrl Pts',(25.9860400862657,45.7223738576064,60.8409540084028)) ;
#7386 = CARTESIAN_POINT('Ctrl Pts',(26.073308227283,45.8755455989771,60.8711208490251)) ;
#7387 = CARTESIAN_POINT('Ctrl Pts',(26.1217552892988,45.9608834226822,60.8884072085208)) ;
#7388 = CARTESIAN_POINT('Ctrl Pts',(26.1983712336257,46.0963466756247,60.9166009893408)) ;
#7389 = CARTESIAN_POINT('Ctrl Pts',(26.2266807713393,46.1464973799217,60.9272060830759)) ;
#7390 = CARTESIAN_POINT('Ctrl Pts',(26.3853710207649,46.4282028809684,60.9877078420715)) ;
#7391 = CARTESIAN_POINT('Ctrl Pts',(26.5143766908135,46.6594344485567,61.0409057065247)) ;
#7392 = CARTESIAN_POINT('Ctrl Pts',(26.6632621942723,46.9296827699029,61.1070233668255)) ;
#7393 = CARTESIAN_POINT('Ctrl Pts',(26.6847644468963,46.968795042416,61.1166890996772)) ;
#7394 = CARTESIAN_POINT('Ctrl Pts',(26.8390184511679,47.2499758749385,61.1868717873152)) ;
#7395 = CARTESIAN_POINT('Ctrl Pts',(26.969967923605,47.491854191672,61.2509483646101)) ;
#7396 = CARTESIAN_POINT('Ctrl Pts',(27.2490607324932,48.0143150857781,61.397343778151)) ;
#7397 = CARTESIAN_POINT('Ctrl Pts',(27.396430725844,48.2952954282289,61.4808850637674)) ;
#7398 = CARTESIAN_POINT('Ctrl Pts',(27.5496308033829,48.5931204307081,61.5744432491943)) ;
#7399 = CARTESIAN_POINT('Ctrl Pts',(27.5583656313921,48.6101204742725,61.5798012478732)) ;
#7400 = CARTESIAN_POINT('Ctrl Pts',(27.7025370493161,48.891036215033,61.6686290067572)) ;
#7401 = CARTESIAN_POINT('Ctrl Pts',(27.8355404157494,49.1549226796748,61.7563011398068)) ;
#7402 = CARTESIAN_POINT('Ctrl Pts',(27.9686046174867,49.4249376060055,61.8499871777608)) ;
#7403 = CARTESIAN_POINT('Ctrl Pts',(27.9714928098665,49.4308011237539,61.8520235913532)) ;
#7404 = CARTESIAN_POINT('Ctrl Pts',(28.1073185789858,49.7066812295575,61.9479300993227)) ;
#7405 = CARTESIAN_POINT('Ctrl Pts',(28.2374330061678,49.9768666464288,62.0460374326432)) ;
#7406 = CARTESIAN_POINT('Ctrl Pts',(28.3670465485902,50.252704329167,62.150317347732)) ;
#7407 = CARTESIAN_POINT('Ctrl Pts',(28.3695621457808,50.2580605419637,62.1523438352739)) ;
#7408 = CARTESIAN_POINT('Ctrl Pts',(28.4965433518478,50.5285623062338,62.2547661851058)) ;
#7409 = CARTESIAN_POINT('Ctrl Pts',(28.6179571450043,50.794089282034,62.3590112370404)) ;
#7410 = CARTESIAN_POINT('Ctrl Pts',(28.7437567626043,51.0767673302899,62.4739538912658)) ;
#7411 = CARTESIAN_POINT('Ctrl Pts',(28.7511947182076,51.0935097128497,62.4807764467365)) ;
#7412 = CARTESIAN_POINT('Ctrl Pts',(28.8213209690217,51.2516332986659,62.5453515762971)) ;
#7413 = CARTESIAN_POINT('Ctrl Pts',(28.8831980925262,51.3931664826133,62.6042351612115)) ;
#7414 = CARTESIAN_POINT('Ctrl Pts',(28.9927392868846,51.6479675595721,62.7119639549746)) ;
#7415 = CARTESIAN_POINT('Ctrl Pts',(29.0407823804013,51.761231940684,62.7604712205008)) ;
#7416 = CARTESIAN_POINT('Ctrl Pts',(29.0999524386712,51.9026374456286,62.8218017972563)) ;
#7417 = CARTESIAN_POINT('Ctrl Pts',(29.1117004986403,51.9308091085127,62.8340587121007)) ;
#7418 = CARTESIAN_POINT('Ctrl Pts',(29.2409148910853,52.2417252333157,62.9697539796517)) ;
#7419 = CARTESIAN_POINT('Ctrl Pts',(29.3543479666627,52.5241195492494,63.0969791494064)) ;
#7420 = CARTESIAN_POINT('Ctrl Pts',(29.5529056802919,53.0381974993347,63.3349410676277)) ;
#7421 = CARTESIAN_POINT('Ctrl Pts',(29.6393958238015,53.2697333986876,63.4444393238498)) ;
#7422 = CARTESIAN_POINT('Ctrl Pts',(29.7413330349859,53.552225996692,63.5808721174967)) ;
#7423 = CARTESIAN_POINT('Ctrl Pts',(29.7595762333489,53.6031771340243,63.6055921287614)) ;
#7424 = CARTESIAN_POINT('Ctrl Pts',(29.8558751791141,53.8742457620922,63.7377058663455)) ;
#7425 = CARTESIAN_POINT('Ctrl Pts',(29.9313616882554,54.0945463050605,63.8470320121601)) ;
#7426 = CARTESIAN_POINT('Ctrl Pts',(30.0246196339593,54.3774106831917,63.9897636197812)) ;
#7427 = CARTESIAN_POINT('Ctrl Pts',(30.044986179155,54.4398806254201,64.0214329924024)) ;
#7428 = CARTESIAN_POINT('Ctrl Pts',(30.1325125522462,54.711432139291,64.1597267018904)) ;
#7429 = CARTESIAN_POINT('Ctrl Pts',(30.197395884353,54.9205828276718,64.2679757139459)) ;
#7430 = CARTESIAN_POINT('Ctrl Pts',(30.2814951271688,55.2033684329563,64.4163117644225)) ;
#7431 = CARTESIAN_POINT('Ctrl Pts',(30.3031271039968,55.2772338818111,64.4552407854699)) ;
#7432 = CARTESIAN_POINT('Ctrl Pts',(30.3813145103917,55.5485088102159,64.5988369765006)) ;
#7433 = CARTESIAN_POINT('Ctrl Pts',(30.4357819827863,55.7457837763599,64.7045566063819)) ;
#7434 = CARTESIAN_POINT('Ctrl Pts',(30.5102987190112,56.0282588904766,64.8576993333359)) ;
#7435 = CARTESIAN_POINT('Ctrl Pts',(30.5323283405607,56.1134884206126,64.904136632693)) ;
#7436 = CARTESIAN_POINT('Ctrl Pts',(30.6009132913455,56.3844426290971,65.0524814877124)) ;
#7437 = CARTESIAN_POINT('Ctrl Pts',(30.6456844427088,56.5701302611241,65.1550649798116)) ;
#7438 = CARTESIAN_POINT('Ctrl Pts',(30.7104181164342,56.8526653483016,65.3125514864397)) ;
#7439 = CARTESIAN_POINT('Ctrl Pts',(30.7319926277606,56.9494716030842,65.3667618614678)) ;
#7440 = CARTESIAN_POINT('Ctrl Pts',(30.7906879595627,57.2204413601012,65.5192013282813)) ;
#7441 = CARTESIAN_POINT('Ctrl Pts',(30.8264612285573,57.3946576755349,65.6180227168432)) ;
#7442 = CARTESIAN_POINT('Ctrl Pts',(30.8812470754923,57.6774250653632,65.7794891180073)) ;
#7443 = CARTESIAN_POINT('Ctrl Pts',(30.9014891525821,57.78593964127,65.8417091024842)) ;
#7444 = CARTESIAN_POINT('Ctrl Pts',(30.9258050052165,57.9216227418847,65.9197805890467)) ;
#7445 = CARTESIAN_POINT('Ctrl Pts',(30.9306139332621,57.9487278912589,65.9353936621802)) ;
#7446 = CARTESIAN_POINT('Ctrl Pts',(30.9472893957238,58.0436810159814,65.9901451420611)) ;
#7447 = CARTESIAN_POINT('Ctrl Pts',(30.9589006933603,58.1115399743055,66.029375203218)) ;
#7448 = CARTESIAN_POINT('Ctrl Pts',(30.9758575565952,58.2133484522822,66.0883678261757)) ;
#7449 = CARTESIAN_POINT('Ctrl Pts',(30.981432705011,58.2472850649058,66.1080549429286)) ;
#7450 = CARTESIAN_POINT('Ctrl Pts',(30.9896801854667,58.2981973836579,66.1376218550297)) ;
#7451 = CARTESIAN_POINT('Ctrl Pts',(30.9924101383193,58.3151693899103,66.1474835319424)) ;
#7452 = CARTESIAN_POINT('Ctrl Pts',(30.995859334791,58.3367668565652,66.1600394167404)) ;
#7453 = CARTESIAN_POINT('Ctrl Pts',(30.9965978053812,58.3413999128707,66.1627332693675)) ;
#7454 = CARTESIAN_POINT('Ctrl Pts',(30.9993038725722,58.3584108602041,66.1726255449783)) ;
#7455 = CARTESIAN_POINT('Ctrl Pts',(31.0012638847202,58.370797523339,66.1798314240518)) ;
#7456 = CARTESIAN_POINT('Ctrl Pts',(31.0031926666446,58.3830508753323,66.1869623392087)) ;
#7457 = CARTESIAN_POINT('',(49.6868966603789,58.3831162793798,61.3897862372794)) ;
#7458 = CARTESIAN_POINT('Ctrl Pts',(31.00318876339,58.3830900980198,66.1869470825038)) ;
#7459 = CARTESIAN_POINT('Ctrl Pts',(34.1171400804529,58.383105259385,65.3874202747358)) ;
#7460 = CARTESIAN_POINT('Ctrl Pts',(37.2310913975658,58.3831073991803,64.5878934669549)) ;
#7461 = CARTESIAN_POINT('Ctrl Pts',(43.4589940299001,58.3831134572106,62.9888398518788)) ;
#7462 = CARTESIAN_POINT('Ctrl Pts',(46.5729453451396,58.3831150235129,62.1893130445791)) ;
#7463 = CARTESIAN_POINT('Ctrl Pts',(49.6868966603789,58.3831162793797,61.3897862372793)) ;
#7464 = CARTESIAN_POINT('',(54.0631310962388,55.1047242171091,51.2065390655857)) ;
#7465 = CARTESIAN_POINT('Ctrl Pts',(49.6868966603789,58.3831162793797,61.3897862372793)) ;
#7466 = CARTESIAN_POINT('Ctrl Pts',(50.2581195512456,58.3831165097558,61.2431211266348)) ;
#7467 = CARTESIAN_POINT('Ctrl Pts',(50.8072353354247,58.3477204548742,61.0251267819229)) ;
#7468 = CARTESIAN_POINT('Ctrl Pts',(51.9220081649887,58.2097833704152,60.4116400136406)) ;
#7469 = CARTESIAN_POINT('Ctrl Pts',(52.4670772856615,58.0979491851444,59.9965228800265)) ;
#7470 = CARTESIAN_POINT('Ctrl Pts',(53.5816676879437,57.7707078254696,58.8613539461653)) ;
#7471 = CARTESIAN_POINT('Ctrl Pts',(54.0821618785496,57.5360202457534,58.095728852092)) ;
#7472 = CARTESIAN_POINT('Ctrl Pts',(54.7917779132289,56.9856758817168,56.3656833294583)) ;
#7473 = CARTESIAN_POINT('Ctrl Pts',(54.9665090756242,56.6687344805943,55.4052128724977)) ;
#7474 = CARTESIAN_POINT('Ctrl Pts',(54.9304672122228,56.1294192803767,53.8587960473992)) ;
#7475 = CARTESIAN_POINT('Ctrl Pts',(54.8428115777871,55.9194276565172,53.2765902560065)) ;
#7476 = CARTESIAN_POINT('Ctrl Pts',(54.5365399857756,55.5068628236254,52.1882811657281)) ;
#7477 = CARTESIAN_POINT('Ctrl Pts',(54.3279790102755,55.3059550653477,51.6825934226883)) ;
#7478 = CARTESIAN_POINT('Ctrl Pts',(54.0631310962388,55.104724217109,51.2065390655857)) ;
#7479 = CARTESIAN_POINT('',(42.1626405421888,48.6398835186857,38.6271207819479)) ;
#7480 = CARTESIAN_POINT('Ctrl Pts',(42.1626405421888,48.6398835186857,38.6271207819478)) ;
#7481 = CARTESIAN_POINT('Ctrl Pts',(42.5377822297253,48.8038201453524,38.8639658740149)) ;
#7482 = CARTESIAN_POINT('Ctrl Pts',(42.9067999896793,48.9676174488035,39.1102437175222)) ;
#7483 = CARTESIAN_POINT('Ctrl Pts',(44.2527377631881,49.5650439193917,40.0085057751427)) ;
#7484 = CARTESIAN_POINT('Ctrl Pts',(45.5100528370125,50.16247038998,41.0271234754859)) ;
#7485 = CARTESIAN_POINT('Ctrl Pts',(46.7673679108369,50.7598968605682,42.0457411758291)) ;
#7486 = CARTESIAN_POINT('Ctrl Pts',(47.9253333160839,51.3573233311564,43.1760240318301)) ;
#7487 = CARTESIAN_POINT('Ctrl Pts',(49.0832987213308,51.9547498017447,44.3063068878311)) ;
#7488 = CARTESIAN_POINT('Ctrl Pts',(50.1320351054498,52.5521762723329,45.5386117246891)) ;
#7489 = CARTESIAN_POINT('Ctrl Pts',(51.1807714895688,53.1496027429211,46.770916561547)) ;
#7490 = CARTESIAN_POINT('Ctrl Pts',(52.1113314035046,53.7470292135094,48.0947297888923)) ;
#7491 = CARTESIAN_POINT('Ctrl Pts',(53.0418913174403,54.3444556840976,49.4185430162376)) ;
#7492 = CARTESIAN_POINT('Ctrl Pts',(53.8463355521134,54.9418821546858,50.8225703263779)) ;
#7493 = CARTESIAN_POINT('Ctrl Pts',(53.9559426933193,55.0232827101246,51.0138718647649)) ;
#7494 = CARTESIAN_POINT('Ctrl Pts',(54.0631310962388,55.1047242171091,51.2065390655857)) ;
#7495 = CARTESIAN_POINT('Ctrl Pts',(42.1626405421888,48.6398835186857,38.6271207819478)) ;
#7496 = CARTESIAN_POINT('Ctrl Pts',(41.7048656670768,48.4398362531006,38.3381053617905)) ;
#7497 = CARTESIAN_POINT('Ctrl Pts',(41.2147380839232,48.2402511664186,38.1029380979704)) ;
#7498 = CARTESIAN_POINT('Ctrl Pts',(40.1532298521113,47.8311033708305,37.7379112181705)) ;
#7499 = CARTESIAN_POINT('Ctrl Pts',(39.581810011503,47.6231195575043,37.6177136594679)) ;
#7500 = CARTESIAN_POINT('Ctrl Pts',(38.0454077153629,47.0862679673289,37.4910821825243)) ;
#7501 = CARTESIAN_POINT('Ctrl Pts',(37.0765536712975,46.7703269230101,37.6087916756144)) ;
#7502 = CARTESIAN_POINT('Ctrl Pts',(35.3073691230138,46.2216256025067,38.2152157232851)) ;
#7503 = CARTESIAN_POINT('Ctrl Pts',(34.5136933172468,45.987905739686,38.6696648884542)) ;
#7504 = CARTESIAN_POINT('Ctrl Pts',(33.3188969657845,45.6640068127921,39.7118246364103)) ;
#7505 = CARTESIAN_POINT('Ctrl Pts',(32.8755155146971,45.5539383581279,40.2266046313311)) ;
#7506 = CARTESIAN_POINT('Ctrl Pts',(32.1996537162509,45.4179657700952,41.2939599752307)) ;
#7507 = CARTESIAN_POINT('Ctrl Pts',(31.9494597369605,45.3830586252741,41.8253945852044)) ;
#7508 = CARTESIAN_POINT('Ctrl Pts',(31.768269675766,45.3830586252741,42.3830402536426)) ;
#7509 = CARTESIAN_POINT('Origin',(38.4256652898321,45.3822493559848,44.5461592142672)) ;
#7510 = CARTESIAN_POINT('',(42.1626405421888,45.3822493559848,38.6271207819479)) ;
#7511 = CARTESIAN_POINT('Origin',(23.47768801576,45.3822493559848,68.2224337400008)) ;
#7512 = CARTESIAN_POINT('',(54.0631310962388,45.3822493559848,51.2065390655857)) ;
#7513 = CARTESIAN_POINT('Origin',(47.9460674476988,45.3822493559848,54.6097041100275)) ;
#7514 = CARTESIAN_POINT('',(49.6868966603788,45.3822493559848,61.3897862372794)) ;
#7515 = CARTESIAN_POINT('Origin',(30.7171869358834,45.3822493559848,66.2603798709065)) ;
#7516 = CARTESIAN_POINT('Ctrl Pts',(30.8134080024022,57.8271591829153,66.2356745000382)) ;
#7517 = CARTESIAN_POINT('Ctrl Pts',(30.8134911684381,57.8726762309135,66.2356531466295)) ;
#7518 = CARTESIAN_POINT('Ctrl Pts',(30.8175149348243,57.9189559198363,66.2346200189886)) ;
#7519 = CARTESIAN_POINT('Ctrl Pts',(30.8339069695655,58.0070760891654,66.2304112598029)) ;
#7520 = CARTESIAN_POINT('Ctrl Pts',(30.8464719817728,58.051172006285,66.2271851130226)) ;
#7521 = CARTESIAN_POINT('Ctrl Pts',(30.8814813724371,58.1280396083484,66.2181962292831)) ;
#7522 = CARTESIAN_POINT('Ctrl Pts',(30.9017034964742,58.1581206857625,66.2130040703033)) ;
#7523 = CARTESIAN_POINT('Ctrl Pts',(30.9363795480004,58.1912258389426,66.2041007735077)) ;
#7524 = CARTESIAN_POINT('Ctrl Pts',(30.9500225532736,58.2011509267379,66.200597845129)) ;
#7525 = CARTESIAN_POINT('Ctrl Pts',(30.9779076696627,58.2136664809671,66.1934381641254)) ;
#7526 = CARTESIAN_POINT('Ctrl Pts',(30.9913762520981,58.2169696033494,66.1899800199146)) ;
#7527 = CARTESIAN_POINT('Ctrl Pts',(31.005319018212,58.2172758076354,66.1864001260282)) ;
#7528 = CARTESIAN_POINT('Ctrl Pts',(31.0031885544775,58.3830247512579,66.1869471361434)) ;
#7529 = CARTESIAN_POINT('Ctrl Pts',(30.9963789496716,58.3830247228379,66.1886955454916)) ;
#7530 = CARTESIAN_POINT('Ctrl Pts',(30.9896247806473,58.3837424765067,66.1904297213503)) ;
#7531 = CARTESIAN_POINT('Ctrl Pts',(30.9758330390786,58.3866521090712,66.1939708387241)) ;
#7532 = CARTESIAN_POINT('Ctrl Pts',(30.9689139763115,58.3889169428641,66.1957473521001)) ;
#7533 = CARTESIAN_POINT('Ctrl Pts',(30.9468729562285,58.3985444430763,66.2014065242041)) ;
#7534 = CARTESIAN_POINT('Ctrl Pts',(30.9330378733326,58.4085611720431,66.2049587697639)) ;
#7535 = CARTESIAN_POINT('Ctrl Pts',(30.8990356285796,58.4411881110303,66.2136890623845)) ;
#7536 = CARTESIAN_POINT('Ctrl Pts',(30.8795612593899,58.4701790972771,66.2186892305213)) ;
#7537 = CARTESIAN_POINT('Ctrl Pts',(30.8454692246162,58.5450324121023,66.2274425773009)) ;
#7538 = CARTESIAN_POINT('Ctrl Pts',(30.8332143405224,58.5884045335537,66.2305890968203)) ;
#7539 = CARTESIAN_POINT('Ctrl Pts',(30.8172539293367,58.675275268205,66.2346870339127)) ;
#7540 = CARTESIAN_POINT('Ctrl Pts',(30.8134073328871,58.721038685519,66.2356746719405)) ;
#7541 = CARTESIAN_POINT('Ctrl Pts',(30.8134076051844,58.7660385537515,66.2356746020264)) ;
#7542 = CARTESIAN_POINT('Ctrl Pts',(31.0173239967825,58.2943663992286,66.2313141867391)) ;
#7543 = CARTESIAN_POINT('Ctrl Pts',(30.8272744005839,58.2924602039142,66.2803148338344)) ;
#7544 = CARTESIAN_POINT('Ctrl Pts',(30.8666087426552,58.191081348463,66.4437121508651)) ;
#7545 = CARTESIAN_POINT('Ctrl Pts',(30.9338538642454,57.7522999682189,65.9152482091109)) ;
#7546 = CARTESIAN_POINT('Ctrl Pts',(30.7458602690527,57.7503889246408,65.9722138304264)) ;
#7547 = CARTESIAN_POINT('Ctrl Pts',(30.7920398310218,57.6489874077046,66.1339482282166)) ;
#7548 = CARTESIAN_POINT('Ctrl Pts',(30.8306212790909,57.21110331024,65.6049265502847)) ;
#7549 = CARTESIAN_POINT('Ctrl Pts',(30.6451794827466,57.2091968025836,65.6697195946995)) ;
#7550 = CARTESIAN_POINT('Ctrl Pts',(30.6981068121273,57.1078632090985,65.8294151776596)) ;
#7551 = CARTESIAN_POINT('Ctrl Pts',(30.6474937677951,56.3997926693554,65.1514197248828)) ;
#7552 = CARTESIAN_POINT('Ctrl Pts',(30.4665934227563,56.3978864499735,65.227653528776)) ;
#7553 = CARTESIAN_POINT('Ctrl Pts',(30.5293754831954,56.2965290899915,65.3836047172742)) ;
#7554 = CARTESIAN_POINT('Ctrl Pts',(30.581679313116,56.1295297083734,65.0020936671592)) ;
#7555 = CARTESIAN_POINT('Ctrl Pts',(30.4024119119524,56.1276240321184,65.0820955068002)) ;
#7556 = CARTESIAN_POINT('Ctrl Pts',(30.4684307812205,56.0262125668428,65.2366705986467)) ;
#7557 = CARTESIAN_POINT('Ctrl Pts',(30.4407980320214,55.5885108130536,64.7078405549652)) ;
#7558 = CARTESIAN_POINT('Ctrl Pts',(30.2650353509719,55.5866055506174,64.7952692923242)) ;
#7559 = CARTESIAN_POINT('Ctrl Pts',(30.3374787224399,55.485272016298,64.9469891274856)) ;
#7560 = CARTESIAN_POINT('Ctrl Pts',(30.3657746842047,55.3179011606876,64.5629812644996)) ;
#7561 = CARTESIAN_POINT('Ctrl Pts',(30.1918780290501,55.3159940909446,64.6540658012614)) ;
#7562 = CARTESIAN_POINT('Ctrl Pts',(30.2674776517272,55.2146518759856,64.8042324556393)) ;
#7563 = CARTESIAN_POINT('Ctrl Pts',(30.2065304249104,54.7764805321232,64.2778126981827)) ;
#7564 = CARTESIAN_POINT('Ctrl Pts',(30.0365957838312,54.7745728258419,64.3760973749008)) ;
#7565 = CARTESIAN_POINT('Ctrl Pts',(30.118383848403,54.673110454093,64.5229064486545)) ;
#7566 = CARTESIAN_POINT('Ctrl Pts',(30.1222957661658,54.5052712784508,64.137525239918)) ;
#7567 = CARTESIAN_POINT('Ctrl Pts',(29.954464616695,54.5033650628297,64.2393538637961)) ;
#7568 = CARTESIAN_POINT('Ctrl Pts',(30.0393485098831,54.4020271817821,64.3844774616171)) ;
#7569 = CARTESIAN_POINT('Ctrl Pts',(29.9455876310585,53.9638812711027,63.8631253385711)) ;
#7570 = CARTESIAN_POINT('Ctrl Pts',(29.7821625432364,53.9619749130418,63.9718859746674)) ;
#7571 = CARTESIAN_POINT('Ctrl Pts',(29.873035343762,53.860610246182,64.113318337735)) ;
#7572 = CARTESIAN_POINT('Ctrl Pts',(29.8529205076406,53.6935003224001,63.7286963367937)) ;
#7573 = CARTESIAN_POINT('Ctrl Pts',(29.691807035817,53.6915946088883,63.8408543226021)) ;
#7574 = CARTESIAN_POINT('Ctrl Pts',(29.7856090795231,53.5901950776356,63.9803370049613)) ;
#7575 = CARTESIAN_POINT('Ctrl Pts',(29.6594824549092,53.1525885953591,63.4661043934883)) ;
#7576 = CARTESIAN_POINT('Ctrl Pts',(29.503200788466,53.1506832358119,63.5848997167274)) ;
#7577 = CARTESIAN_POINT('Ctrl Pts',(29.6027738980047,53.0493503316824,63.7203702363143)) ;
#7578 = CARTESIAN_POINT('Ctrl Pts',(29.5587376511048,52.8821999703706,63.3379585752569)) ;
#7579 = CARTESIAN_POINT('Ctrl Pts',(29.4049714652684,52.8802927777264,63.4599930285515)) ;
#7580 = CARTESIAN_POINT('Ctrl Pts',(29.5073500068726,52.7789455602911,63.5933458219226)) ;
#7581 = CARTESIAN_POINT('Ctrl Pts',(29.3491929541791,52.3415574725492,63.0879698629551)) ;
#7582 = CARTESIAN_POINT('Ctrl Pts',(29.2006595660773,52.3396495857196,63.216327225387)) ;
#7583 = CARTESIAN_POINT('Ctrl Pts',(29.3084773791931,52.2381712237465,63.3452240787661)) ;
#7584 = CARTESIAN_POINT('Ctrl Pts',(29.2404444313661,52.0708923183226,62.9662055967095)) ;
#7585 = CARTESIAN_POINT('Ctrl Pts',(29.0946348929149,52.0689860210687,63.0976434808219)) ;
#7586 = CARTESIAN_POINT('Ctrl Pts',(29.2051790309548,51.967651026395,63.2243189994837)) ;
#7587 = CARTESIAN_POINT('Ctrl Pts',(29.0154772528091,51.5294526417487,62.7296936231344)) ;
#7588 = CARTESIAN_POINT('Ctrl Pts',(28.8752935944966,51.5275461441804,62.8671172871891)) ;
#7589 = CARTESIAN_POINT('Ctrl Pts',(28.9910265495215,51.4261734610189,62.9890407201091)) ;
#7590 = CARTESIAN_POINT('Ctrl Pts',(28.8990062710636,51.2584285629436,62.6147037460552)) ;
#7591 = CARTESIAN_POINT('Ctrl Pts',(28.761736858127,51.2565228089791,62.755039072442)) ;
#7592 = CARTESIAN_POINT('Ctrl Pts',(28.8799958936779,51.155134072336,62.8745009981941)) ;
#7593 = CARTESIAN_POINT('Ctrl Pts',(28.6595364145706,50.7168256230159,62.3927027901548)) ;
#7594 = CARTESIAN_POINT('Ctrl Pts',(28.5282629209368,50.7149201642748,62.5386603231389)) ;
#7595 = CARTESIAN_POINT('Ctrl Pts',(28.6514413554663,50.6135869790364,62.6530898469933)) ;
#7596 = CARTESIAN_POINT('Ctrl Pts',(28.5364906257386,50.4462620313617,62.2856173447484)) ;
#7597 = CARTESIAN_POINT('Ctrl Pts',(28.4082966641083,50.4443547062453,62.4342875276819)) ;
#7598 = CARTESIAN_POINT('Ctrl Pts',(28.5338335609057,50.343001553274,62.5461074002847)) ;
#7599 = CARTESIAN_POINT('Ctrl Pts',(28.283795141269,49.905609988286,62.0792556818166)) ;
#7600 = CARTESIAN_POINT('Ctrl Pts',(28.1619262162133,49.9037019096497,62.2331580132732)) ;
#7601 = CARTESIAN_POINT('Ctrl Pts',(28.291967471768,49.8022062837453,62.3395771372856)) ;
#7602 = CARTESIAN_POINT('Ctrl Pts',(28.1542570098572,49.635040821776,61.9800832945457)) ;
#7603 = CARTESIAN_POINT('Ctrl Pts',(28.0356389821241,49.6331344367361,62.1364995516978)) ;
#7604 = CARTESIAN_POINT('Ctrl Pts',(28.167949142981,49.5318014383422,62.2402351417232)) ;
#7605 = CARTESIAN_POINT('Ctrl Pts',(27.8892785686591,49.0942250306864,61.7900845915201)) ;
#7606 = CARTESIAN_POINT('Ctrl Pts',(27.7772999871363,49.0923183862306,61.9513222262773)) ;
#7607 = CARTESIAN_POINT('Ctrl Pts',(27.9138077417617,48.9909365753663,62.0494205950826)) ;
#7608 = CARTESIAN_POINT('Ctrl Pts',(27.7536506015481,48.8238179925643,61.6991333239323)) ;
#7609 = CARTESIAN_POINT('Ctrl Pts',(27.6450725909719,48.8219121926736,61.8626802565342)) ;
#7610 = CARTESIAN_POINT('Ctrl Pts',(27.7836051589675,48.7205331729861,61.9579007407528)) ;
#7611 = CARTESIAN_POINT('Ctrl Pts',(27.4769725624454,48.2823982252869,61.5259407616695)) ;
#7612 = CARTESIAN_POINT('Ctrl Pts',(27.375333692239,48.2804926624883,61.6938867971212)) ;
#7613 = CARTESIAN_POINT('Ctrl Pts',(27.5177502752558,48.17915824216,61.7832417812041)) ;
#7614 = CARTESIAN_POINT('Ctrl Pts',(27.3358290336846,48.0114576298707,61.4436323948175)) ;
#7615 = CARTESIAN_POINT('Ctrl Pts',(27.2377262624136,48.009552069624,61.6136730295645)) ;
#7616 = CARTESIAN_POINT('Ctrl Pts',(27.381907086481,47.9080609643674,61.6999779551815)) ;
#7617 = CARTESIAN_POINT('Ctrl Pts',(27.0484326317699,47.4697670851943,61.2879435657883)) ;
#7618 = CARTESIAN_POINT('Ctrl Pts',(26.9575440003344,47.4678622559094,61.4619430611764)) ;
#7619 = CARTESIAN_POINT('Ctrl Pts',(27.105282807758,47.3665093096313,61.542170867765)) ;
#7620 = CARTESIAN_POINT('Ctrl Pts',(26.9025922094126,47.1991192501543,61.2147751017004)) ;
#7621 = CARTESIAN_POINT('Ctrl Pts',(26.8153628578287,47.1972127705413,61.3906367503116)) ;
#7622 = CARTESIAN_POINT('Ctrl Pts',(26.96475857933,47.0958808569866,61.4677612275413)) ;
#7623 = CARTESIAN_POINT('Ctrl Pts',(26.6066553014126,46.6582159321358,61.0777276907649)) ;
#7624 = CARTESIAN_POINT('Ctrl Pts',(26.5268521641293,46.6563091332017,61.2570830605992)) ;
#7625 = CARTESIAN_POINT('Ctrl Pts',(26.6793104751995,46.5549171221787,61.3278796940087)) ;
#7626 = CARTESIAN_POINT('Ctrl Pts',(26.4564442172867,46.3878930438346,61.0138098095528)) ;
#7627 = CARTESIAN_POINT('Ctrl Pts',(26.3804132190556,46.3859871917477,61.1947958430729)) ;
#7628 = CARTESIAN_POINT('Ctrl Pts',(26.5343309437764,46.284617201445,61.2623921487697)) ;
#7629 = CARTESIAN_POINT('Ctrl Pts',(26.1525452484292,45.847008993639,60.8956077330631)) ;
#7630 = CARTESIAN_POINT('Ctrl Pts',(26.0841461601336,45.8451033188968,61.0796128500728)) ;
#7631 = CARTESIAN_POINT('Ctrl Pts',(26.2407723084679,45.7437666877396,61.1407241912794)) ;
#7632 = CARTESIAN_POINT('Ctrl Pts',(25.9987670923634,45.5765948766442,60.8412757218746)) ;
#7633 = CARTESIAN_POINT('Ctrl Pts',(25.9342268983673,45.5746876691494,61.0266727188793)) ;
#7634 = CARTESIAN_POINT('Ctrl Pts',(26.0920704394477,45.4732994150099,61.0844840121749)) ;
#7635 = CARTESIAN_POINT('Ctrl Pts',(25.8432056478439,45.3060601767044,60.7917538220346)) ;
#7636 = CARTESIAN_POINT('Ctrl Pts',(25.7825741591705,45.3041537286489,60.9784198972454)) ;
#7637 = CARTESIAN_POINT('Ctrl Pts',(25.9415364981948,45.2027271666488,61.0328961571237)) ;
#7638 = CARTESIAN_POINT('Ctrl Pts',(25.6853615766559,45.1993067880442,60.7456299070416)) ;
#7639 = CARTESIAN_POINT('Ctrl Pts',(25.629734117304,45.2022941676425,60.9315956388122)) ;
#7640 = CARTESIAN_POINT('Ctrl Pts',(25.4693419487448,45.3026134137914,60.8880411536154)) ;
#7641 = CARTESIAN_POINT('Ctrl Pts',(25.8489500846755,45.4820412744461,60.7939313563783)) ;
#7642 = CARTESIAN_POINT('Ctrl Pts',(25.7892537891377,45.4850270680332,60.9786815820694)) ;
#7643 = CARTESIAN_POINT('Ctrl Pts',(25.629811962671,45.5853439255465,60.9316167777176)) ;
#7644 = CARTESIAN_POINT('Ctrl Pts',(26.0105939396619,45.7643410734543,60.8475011219934)) ;
#7645 = CARTESIAN_POINT('Ctrl Pts',(25.9468763160639,45.7673274764264,61.0308984687925)) ;
#7646 = CARTESIAN_POINT('Ctrl Pts',(25.7884565009027,45.8675609242035,60.9803505370629)) ;
#7647 = CARTESIAN_POINT('Ctrl Pts',(26.3294012120924,46.3280183067159,60.9648183695104)) ;
#7648 = CARTESIAN_POINT('Ctrl Pts',(26.2577565707799,46.3310049155992,61.1452672008741)) ;
#7649 = CARTESIAN_POINT('Ctrl Pts',(26.1016975009351,46.4312549192417,61.0878703804171)) ;
#7650 = CARTESIAN_POINT('Ctrl Pts',(26.4867761257954,46.6093355962199,61.0286488460598)) ;
#7651 = CARTESIAN_POINT('Ctrl Pts',(26.411218900482,46.6123217179453,61.2074961609377)) ;
#7652 = CARTESIAN_POINT('Ctrl Pts',(26.2564710038353,46.7126174787322,61.1467238390184)) ;
#7653 = CARTESIAN_POINT('Ctrl Pts',(26.7966466733539,47.1717937444952,61.1662561586161)) ;
#7654 = CARTESIAN_POINT('Ctrl Pts',(26.7133853291535,47.1747789756452,61.3416468164381)) ;
#7655 = CARTESIAN_POINT('Ctrl Pts',(26.5613882158301,47.2750030883802,61.2741894600574)) ;
#7656 = CARTESIAN_POINT('Ctrl Pts',(26.9490977408211,47.452783888214,61.2399992875839)) ;
#7657 = CARTESIAN_POINT('Ctrl Pts',(26.8620488448114,47.4557718391357,61.4135417477089)) ;
#7658 = CARTESIAN_POINT('Ctrl Pts',(26.7115606656982,47.5560106522166,61.3428015600556)) ;
#7659 = CARTESIAN_POINT('Ctrl Pts',(27.2490465430224,48.0142871287605,61.3973346389138)) ;
#7660 = CARTESIAN_POINT('Ctrl Pts',(27.1545450044284,48.0172768213532,61.5669393649232)) ;
#7661 = CARTESIAN_POINT('Ctrl Pts',(27.0073417659582,48.1176560532207,61.4897659440178)) ;
#7662 = CARTESIAN_POINT('Ctrl Pts',(27.3964165763424,48.2952668191079,61.4808751506582)) ;
#7663 = CARTESIAN_POINT('Ctrl Pts',(27.2982508531111,48.298253523814,61.6483796930605)) ;
#7664 = CARTESIAN_POINT('Ctrl Pts',(27.1526809617576,48.3984774868501,61.5679867097387)) ;
#7665 = CARTESIAN_POINT('Ctrl Pts',(27.6853561273312,48.8569739450404,61.6573296331633)) ;
#7666 = CARTESIAN_POINT('Ctrl Pts',(27.5800124452371,48.8599612929924,61.8204175090139)) ;
#7667 = CARTESIAN_POINT('Ctrl Pts',(27.4380946261539,48.9602369846067,61.7337961393913)) ;
#7668 = CARTESIAN_POINT('Ctrl Pts',(27.8271307922781,49.1378578224168,61.7503802179487)) ;
#7669 = CARTESIAN_POINT('Ctrl Pts',(27.7182647454188,49.1408439739518,61.9111378886765)) ;
#7670 = CARTESIAN_POINT('Ctrl Pts',(27.5782584466766,49.2411084826924,61.8214479697392)) ;
#7671 = CARTESIAN_POINT('Ctrl Pts',(28.1042995146782,49.7002903801074,61.945525014867)) ;
#7672 = CARTESIAN_POINT('Ctrl Pts',(27.988549523697,49.7032760750881,62.1013977581118)) ;
#7673 = CARTESIAN_POINT('Ctrl Pts',(27.8525562927794,49.8035038746615,62.0056963119981)) ;
#7674 = CARTESIAN_POINT('Ctrl Pts',(28.2397716087933,49.981574104122,62.0476554027074)) ;
#7675 = CARTESIAN_POINT('Ctrl Pts',(28.1206577488799,49.9845603797024,62.2009788340381)) ;
#7676 = CARTESIAN_POINT('Ctrl Pts',(27.9868394128148,50.0849206295178,62.1023846910028)) ;
#7677 = CARTESIAN_POINT('Ctrl Pts',(28.5043816473993,50.5452598054824,62.2610884821112)) ;
#7678 = CARTESIAN_POINT('Ctrl Pts',(28.3786978494748,50.5482445256917,62.4090687367887)) ;
#7679 = CARTESIAN_POINT('Ctrl Pts',(28.2492480466419,50.6484794514239,62.3046924854854)) ;
#7680 = CARTESIAN_POINT('Ctrl Pts',(28.6332388724747,50.8275371605559,62.3721571464137)) ;
#7681 = CARTESIAN_POINT('Ctrl Pts',(28.5043578421195,50.8305243024046,62.5173611292313)) ;
#7682 = CARTESIAN_POINT('Ctrl Pts',(28.3772112458526,50.9307473367347,62.4101803139267)) ;
#7683 = CARTESIAN_POINT('Ctrl Pts',(28.821311272216,51.2516112326398,62.5453424745609)) ;
#7684 = CARTESIAN_POINT('Ctrl Pts',(28.6877625818993,51.2545984104365,62.6862205204475)) ;
#7685 = CARTESIAN_POINT('Ctrl Pts',(28.5642488700406,51.3548887142751,62.574973858029)) ;
#7686 = CARTESIAN_POINT('Ctrl Pts',(28.8831921134199,51.3931523912284,62.6042291234362)) ;
#7687 = CARTESIAN_POINT('Ctrl Pts',(28.748107618006,51.3961391935655,62.7436360358572)) ;
#7688 = CARTESIAN_POINT('Ctrl Pts',(28.6258271935325,51.4964465475109,62.6310493654478)) ;
#7689 = CARTESIAN_POINT('Ctrl Pts',(29.0048607208363,51.6761627264484,62.7238846652)) ;
#7690 = CARTESIAN_POINT('Ctrl Pts',(28.8667575141589,51.679148867895,62.8602991907019)) ;
#7691 = CARTESIAN_POINT('Ctrl Pts',(28.7469484326335,51.7794030062205,62.7450428577575)) ;
#7692 = CARTESIAN_POINT('Ctrl Pts',(29.0646528837623,51.8176028378186,62.7846512653971)) ;
#7693 = CARTESIAN_POINT('Ctrl Pts',(28.9250665124087,51.8205891355625,62.9195470595252)) ;
#7694 = CARTESIAN_POINT('Ctrl Pts',(28.806519466295,51.9208298261689,62.8029822662677)) ;
#7695 = CARTESIAN_POINT('Ctrl Pts',(29.240916523989,52.2417288193202,62.969755415835)) ;
#7696 = CARTESIAN_POINT('Ctrl Pts',(29.096957913189,52.2447151365731,63.1000268989965)) ;
#7697 = CARTESIAN_POINT('Ctrl Pts',(28.9822749700762,52.3449566194198,62.9796178859191)) ;
#7698 = CARTESIAN_POINT('Ctrl Pts',(29.3543526842364,52.5241300049544,63.0969834020191)) ;
#7699 = CARTESIAN_POINT('Ctrl Pts',(29.207580250032,52.5271161388288,63.2240797522907)) ;
#7700 = CARTESIAN_POINT('Ctrl Pts',(29.0955835545825,52.6274277787482,63.1012218259211)) ;
#7701 = CARTESIAN_POINT('Ctrl Pts',(29.5725963126369,53.0891744812499,63.3585368522534)) ;
#7702 = CARTESIAN_POINT('Ctrl Pts',(29.4204136017986,53.0921595377921,63.4790977763337)) ;
#7703 = CARTESIAN_POINT('Ctrl Pts',(29.3138573916988,53.1923844745183,63.3514288365555)) ;
#7704 = CARTESIAN_POINT('Ctrl Pts',(29.6773310089795,53.3716654702982,63.492757098003)) ;
#7705 = CARTESIAN_POINT('Ctrl Pts',(29.5225534466469,53.3746531996277,63.6099685775886)) ;
#7706 = CARTESIAN_POINT('Ctrl Pts',(29.4188136322877,53.474885769066,63.4800061206353)) ;
#7707 = CARTESIAN_POINT('Ctrl Pts',(29.8780214581697,53.9365848433025,63.7680888401132)) ;
#7708 = CARTESIAN_POINT('Ctrl Pts',(29.7182702841382,53.9395741566699,63.8784329849204)) ;
#7709 = CARTESIAN_POINT('Ctrl Pts',(29.6203503545103,54.0399343658536,63.7441201390589)) ;
#7710 = CARTESIAN_POINT('Ctrl Pts',(29.9739226608531,54.2194050938164,63.9091508316086)) ;
#7711 = CARTESIAN_POINT('Ctrl Pts',(29.811797075346,54.2223916876827,64.0159678115517)) ;
#7712 = CARTESIAN_POINT('Ctrl Pts',(29.7167933284806,54.3226177650003,63.8794844435482)) ;
#7713 = CARTESIAN_POINT('Ctrl Pts',(30.1563273052154,54.7853172886129,64.1973543020858)) ;
#7714 = CARTESIAN_POINT('Ctrl Pts',(29.98968524754,54.7883043794054,64.2969811629213)) ;
#7715 = CARTESIAN_POINT('Ctrl Pts',(29.9007532198412,54.888570414198,64.156492633824)) ;
#7716 = CARTESIAN_POINT('Ctrl Pts',(30.2429188259929,55.0683374452683,64.3446637303482)) ;
#7717 = CARTESIAN_POINT('Ctrl Pts',(30.0741333911327,55.0713235720091,64.4406149178796)) ;
#7718 = CARTESIAN_POINT('Ctrl Pts',(29.9883028278047,55.1715968138862,64.2982152529656)) ;
#7719 = CARTESIAN_POINT('Ctrl Pts',(30.4059090570349,55.6338317486017,64.6440003385919)) ;
#7720 = CARTESIAN_POINT('Ctrl Pts',(30.2330926356945,55.6368172834075,64.7324821192857)) ;
#7721 = CARTESIAN_POINT('Ctrl Pts',(30.1535533825065,55.7370429277092,64.5864445252369)) ;
#7722 = CARTESIAN_POINT('Ctrl Pts',(30.4823952983082,55.916215478763,64.7961309034391)) ;
#7723 = CARTESIAN_POINT('Ctrl Pts',(30.3076853561814,55.9192018042982,64.8808238492804)) ;
#7724 = CARTESIAN_POINT('Ctrl Pts',(30.2313935555733,56.0195762764982,64.7331583223123)) ;
#7725 = CARTESIAN_POINT('Ctrl Pts',(30.6254121455451,56.4812254904277,65.1054688516006)) ;
#7726 = CARTESIAN_POINT('Ctrl Pts',(30.4471709208848,56.4842101347963,65.1824414452389)) ;
#7727 = CARTESIAN_POINT('Ctrl Pts',(30.3773704514723,56.5844490941092,65.0315147900252)) ;
#7728 = CARTESIAN_POINT('Ctrl Pts',(30.6917624032461,56.763743935905,65.2622767975204)) ;
#7729 = CARTESIAN_POINT('Ctrl Pts',(30.5118840267287,56.7667309512707,65.3353401301383)) ;
#7730 = CARTESIAN_POINT('Ctrl Pts',(30.4453928475244,56.8669533046602,65.1829163320907)) ;
#7731 = CARTESIAN_POINT('Ctrl Pts',(30.8141613823402,57.3288079962077,65.5801651959044)) ;
#7732 = CARTESIAN_POINT('Ctrl Pts',(30.6312620619075,57.3317959921678,65.6453060803128)) ;
#7733 = CARTESIAN_POINT('Ctrl Pts',(30.5715081411308,57.4320972449782,65.4901649529916)) ;
#7734 = CARTESIAN_POINT('Ctrl Pts',(30.8702287449917,57.6115036703986,65.7413392603775)) ;
#7735 = CARTESIAN_POINT('Ctrl Pts',(30.6859486276515,57.614489922045,65.802459364614)) ;
#7736 = CARTESIAN_POINT('Ctrl Pts',(30.6295920933399,57.7147356136583,65.6460186938791)) ;
#7737 = CARTESIAN_POINT('Ctrl Pts',(30.9716670485772,58.1775332618979,66.0670303867177)) ;
#7738 = CARTESIAN_POINT('Ctrl Pts',(30.7848903419995,58.1805194049524,66.1200320694339)) ;
#7739 = CARTESIAN_POINT('Ctrl Pts',(30.7354281864928,58.2807563670397,65.9612716407878)) ;
#7740 = CARTESIAN_POINT('Ctrl Pts',(31.0170807712485,58.4605262973882,66.2317049895088)) ;
#7741 = CARTESIAN_POINT('Ctrl Pts',(30.8291853189397,58.4635110441295,66.2806047680588)) ;
#7742 = CARTESIAN_POINT('Ctrl Pts',(30.7832293261232,58.5638587343566,66.1208594483691)) ;
#7743 = CARTESIAN_POINT('Ctrl Pts',(31.0569564067032,58.7433256931628,66.3973145222243)) ;
#7744 = CARTESIAN_POINT('Ctrl Pts',(30.868086917137,58.7463119239391,66.4420830740152)) ;
#7745 = CARTESIAN_POINT('Ctrl Pts',(30.8256211934509,58.846513767945,66.281331471652)) ;
#7746 = CARTESIAN_POINT('Origin',(23.47768801576,59.8830586252741,68.2224337400009)) ;
#7747 = CARTESIAN_POINT('Origin',(-4.86729604997798,45.3830586252741,47.6904007594832)) ;
#7748 = CARTESIAN_POINT('',(17.1688739128827,45.3830610445956,63.6388169494918)) ;
#7749 = CARTESIAN_POINT('',(0.569856645481698,45.3830586252741,51.5789200251186)) ;
#7750 = CARTESIAN_POINT('',(17.1688762698447,45.3830586252741,63.6388137054137)) ;
#7751 = CARTESIAN_POINT('Ctrl Pts',(17.1688730549123,45.3830586252741,63.6388181303861)) ;
#7752 = CARTESIAN_POINT('Ctrl Pts',(17.1800590780183,45.3830586252741,63.6469452532392)) ;
#7753 = CARTESIAN_POINT('Ctrl Pts',(17.1921565915667,45.3830586252741,63.6536652985854)) ;
#7754 = CARTESIAN_POINT('Ctrl Pts',(17.2187686671259,45.3830586252741,63.6645720588386)) ;
#7755 = CARTESIAN_POINT('Ctrl Pts',(17.2332205987557,45.3830586252741,63.6684413705484)) ;
#7756 = CARTESIAN_POINT('Ctrl Pts',(17.2748860520113,45.3830586252741,63.6744361969284)) ;
#7757 = CARTESIAN_POINT('Ctrl Pts',(17.3022690103674,45.3830586252741,63.6724758731919)) ;
#7758 = CARTESIAN_POINT('Ctrl Pts',(17.3571375210947,45.3830586252741,63.6583151154743)) ;
#7759 = CARTESIAN_POINT('Ctrl Pts',(17.3840869789834,45.3830586252736,63.6453977385134)) ;
#7760 = CARTESIAN_POINT('Ctrl Pts',(17.4299533045875,45.3830586252736,63.6129782098527)) ;
#7761 = CARTESIAN_POINT('Ctrl Pts',(17.4493637769369,45.3830586252741,63.594256853187)) ;
#7762 = CARTESIAN_POINT('Ctrl Pts',(17.4656808998813,45.3830586252741,63.5731570074722)) ;
#7763 = CARTESIAN_POINT('',(17.1123854551458,45.3830674541108,63.721395608331)) ;
#7764 = CARTESIAN_POINT('Ctrl Pts',(17.1437460237931,45.3830586252741,64.0222933688402)) ;
#7765 = CARTESIAN_POINT('Ctrl Pts',(17.158246936494,45.3830586252741,64.000424741156)) ;
#7766 = CARTESIAN_POINT('Ctrl Pts',(17.1696066385742,45.3830586252745,63.9764616766277)) ;
#7767 = CARTESIAN_POINT('Ctrl Pts',(17.185738799857,45.3830586252745,63.9230452426601)) ;
#7768 = CARTESIAN_POINT('Ctrl Pts',(17.1894694076506,45.3830586252741,63.8933258428105)) ;
#7769 = CARTESIAN_POINT('Ctrl Pts',(17.1855264735452,45.3830586252741,63.8366740578439)) ;
#7770 = CARTESIAN_POINT('Ctrl Pts',(17.1787049287075,45.3830586252741,63.8100195880785)) ;
#7771 = CARTESIAN_POINT('Ctrl Pts',(17.1599065242039,45.3830586252741,63.7725456534273)) ;
#7772 = CARTESIAN_POINT('Ctrl Pts',(17.1518122170667,45.3830586252741,63.7602351390352)) ;
#7773 = CARTESIAN_POINT('Ctrl Pts',(17.1334102581903,45.3830586252741,63.7386874610371)) ;
#7774 = CARTESIAN_POINT('Ctrl Pts',(17.123408783065,45.3830586252741,63.7294110116011)) ;
#7775 = CARTESIAN_POINT('Ctrl Pts',(17.1123823807625,45.3830586252741,63.7213999560576)) ;
#7776 = CARTESIAN_POINT('',(1.4648950896395,45.3830586252741,52.352810316749)) ;
#7777 = CARTESIAN_POINT('',(1.4648950896395,45.3830586252741,52.352810316749)) ;
#7778 = CARTESIAN_POINT('Origin',(5.57939185568678,45.3830586252741,46.6896913561244)) ;
#7779 = CARTESIAN_POINT('Ctrl Pts',(17.4100576973813,45.383050240205,63.814048285042)) ;
#7780 = CARTESIAN_POINT('Ctrl Pts',(17.6138710905714,45.9804808943662,63.5335228327087)) ;
#7781 = CARTESIAN_POINT('Ctrl Pts',(17.8426988440834,46.5779115664506,63.2729997284105)) ;
#7782 = CARTESIAN_POINT('Ctrl Pts',(18.0715249883393,47.1753380370388,63.0124784562693)) ;
#7783 = CARTESIAN_POINT('Ctrl Pts',(18.3234128709904,47.772764507627,62.7741819348792)) ;
#7784 = CARTESIAN_POINT('Ctrl Pts',(18.5753007536416,48.3701909782152,62.5358854134891)) ;
#7785 = CARTESIAN_POINT('Ctrl Pts',(18.8481013560865,48.9676174488035,62.3218467047498)) ;
#7786 = CARTESIAN_POINT('Ctrl Pts',(19.1209019585313,49.5650439193917,62.1078079960104)) ;
#7787 = CARTESIAN_POINT('Ctrl Pts',(19.4122878422165,50.16247038998,61.9198532027167)) ;
#7788 = CARTESIAN_POINT('Ctrl Pts',(19.7036737259018,50.7598968605682,61.731898409423)) ;
#7789 = CARTESIAN_POINT('Ctrl Pts',(20.0111588892076,51.3573233311564,61.5716310956004)) ;
#7790 = CARTESIAN_POINT('Ctrl Pts',(20.3186440525133,51.9547498017447,61.4113637817778)) ;
#7791 = CARTESIAN_POINT('Ctrl Pts',(20.6396051404426,52.5521762723329,61.2801512916392)) ;
#7792 = CARTESIAN_POINT('Ctrl Pts',(20.9605662283718,53.1496027429211,61.1489388015006)) ;
#7793 = CARTESIAN_POINT('Ctrl Pts',(21.29226491409,53.7470292135094,61.0479005937476)) ;
#7794 = CARTESIAN_POINT('Ctrl Pts',(21.6239635998081,54.3444556840976,60.9468623859946)) ;
#7795 = CARTESIAN_POINT('Ctrl Pts',(21.9635699470823,54.9418821546858,60.8768604829906)) ;
#7796 = CARTESIAN_POINT('Ctrl Pts',(22.3031762943565,55.5393086252741,60.8068585799867)) ;
#7797 = CARTESIAN_POINT('Ctrl Pts',(22.6477929015737,56.1367350958623,60.7684902132863)) ;
#7798 = CARTESIAN_POINT('Ctrl Pts',(22.9924095087908,56.7341615664506,60.7301218465859)) ;
#7799 = CARTESIAN_POINT('Ctrl Pts',(23.3390962285664,57.3315880370388,60.7237143615655)) ;
#7800 = CARTESIAN_POINT('Ctrl Pts',(23.6441167020902,57.8572133193466,60.71807695464)) ;
#7801 = CARTESIAN_POINT('Ctrl Pts',(23.948587351244,58.3830758086166,60.7372314170278)) ;
#7802 = CARTESIAN_POINT('Ctrl Pts',(-4.83792013667371,45.383050240205,47.6499682835265)) ;
#7803 = CARTESIAN_POINT('Ctrl Pts',(-3.8867909684531,45.9804808943662,46.3408495059708)) ;
#7804 = CARTESIAN_POINT('Ctrl Pts',(-2.81892811873079,46.5779115664506,45.1250750192457)) ;
#7805 = CARTESIAN_POINT('Ctrl Pts',(-1.75107277886993,47.1753380370388,43.9093090825868)) ;
#7806 = CARTESIAN_POINT('Ctrl Pts',(-0.575595993164432,47.772764507627,42.7972586494332)) ;
#7807 = CARTESIAN_POINT('Ctrl Pts',(0.599880792541069,48.3701909782152,41.6852082162796)) ;
#7808 = CARTESIAN_POINT('Ctrl Pts',(1.872950270617,48.9676174488035,40.6863609088291)) ;
#7809 = CARTESIAN_POINT('Ctrl Pts',(3.14601974869293,49.5650439193917,39.6875136013786)) ;
#7810 = CARTESIAN_POINT('Ctrl Pts',(4.50582053922401,50.16247038998,38.8103912326747)) ;
#7811 = CARTESIAN_POINT('Ctrl Pts',(5.86562132975509,50.7598968605682,37.9332688639709)) ;
#7812 = CARTESIAN_POINT('Ctrl Pts',(7.30055209184877,51.3573233311564,37.1853547327988)) ;
#7813 = CARTESIAN_POINT('Ctrl Pts',(8.73548285394244,51.9547498017447,36.4374406016267)) ;
#7814 = CARTESIAN_POINT('Ctrl Pts',(10.2333012642789,52.5521762723329,35.8251156476465)) ;
#7815 = CARTESIAN_POINT('Ctrl Pts',(11.7311196746153,53.1496027429212,35.2127906936662)) ;
#7816 = CARTESIAN_POINT('Ctrl Pts',(13.2790468746333,53.7470292135094,34.7412790574855)) ;
#7817 = CARTESIAN_POINT('Ctrl Pts',(14.8269740746514,54.3444556840976,34.2697674213048)) ;
#7818 = CARTESIAN_POINT('Ctrl Pts',(16.4118036952644,54.9418821546858,33.9430918739531)) ;
#7819 = CARTESIAN_POINT('Ctrl Pts',(17.9966333158773,55.5393086252741,33.6164163266014)) ;
#7820 = CARTESIAN_POINT('Ctrl Pts',(19.6048441495572,56.1367350958623,33.4373639486663)) ;
#7821 = CARTESIAN_POINT('Ctrl Pts',(21.2130549832371,56.7341615664506,33.2583115707312)) ;
#7822 = CARTESIAN_POINT('Ctrl Pts',(22.8309263421902,57.3315880370388,33.228409973969)) ;
#7823 = CARTESIAN_POINT('Ctrl Pts',(24.2543552186343,57.8572133193466,33.2021020749834)) ;
#7824 = CARTESIAN_POINT('Ctrl Pts',(25.6752182480186,58.3830758086166,33.2914895661267)) ;
#7825 = CARTESIAN_POINT('',(25.0785449650548,58.3353824278239,41.1845908766823)) ;
#7826 = CARTESIAN_POINT('',(23.8674681578449,58.2172712656977,60.4340619665212)) ;
#7827 = CARTESIAN_POINT('Ctrl Pts',(25.0785449650548,58.3353824278239,41.1845908766823)) ;
#7828 = CARTESIAN_POINT('Ctrl Pts',(24.9165967247392,58.3308357083915,43.7586844600685)) ;
#7829 = CARTESIAN_POINT('Ctrl Pts',(24.7350928605288,58.3244410146232,46.6436057862439)) ;
#7830 = CARTESIAN_POINT('Ctrl Pts',(24.423261223575,58.3066351812269,51.6000277530103)) ;
#7831 = CARTESIAN_POINT('Ctrl Pts',(24.0807588371245,58.2895264404745,57.0439473259468)) ;
#7832 = CARTESIAN_POINT('Ctrl Pts',(23.8674708952131,58.2172696107887,60.4340621034685)) ;
#7833 = CARTESIAN_POINT('Ctrl Pts',(23.8674681578449,58.2172712656977,60.4340619665212)) ;
#7834 = CARTESIAN_POINT('Ctrl Pts',(23.7062059304299,57.9495340002374,60.4259926846083)) ;
#7835 = CARTESIAN_POINT('Ctrl Pts',(23.544757653971,57.6819084045905,60.4229408514303)) ;
#7836 = CARTESIAN_POINT('Ctrl Pts',(23.3835363156539,57.4145313636579,60.4248870693006)) ;
#7837 = CARTESIAN_POINT('Ctrl Pts',(23.233875375543,57.166326630167,60.4266937333512)) ;
#7838 = CARTESIAN_POINT('Ctrl Pts',(23.0843664411127,56.9182638872676,60.4328052874967)) ;
#7839 = CARTESIAN_POINT('Ctrl Pts',(22.9352053386692,56.6702295478715,60.4432068221641)) ;
#7840 = CARTESIAN_POINT('Ctrl Pts',(22.9236835498855,56.6510704023381,60.444010277512)) ;
#7841 = CARTESIAN_POINT('Ctrl Pts',(22.9121630148862,56.6319118940957,60.4448393772268)) ;
#7842 = CARTESIAN_POINT('Ctrl Pts',(22.9006438534892,56.6127538456681,60.4456941141314)) ;
#7843 = CARTESIAN_POINT('Ctrl Pts',(22.7495669628603,56.3614909032359,60.4569042178363)) ;
#7844 = CARTESIAN_POINT('Ctrl Pts',(22.5987433261589,56.1103350670462,60.4725243164303)) ;
#7845 = CARTESIAN_POINT('Ctrl Pts',(22.4485236466779,55.8590202585561,60.4925253591705)) ;
#7846 = CARTESIAN_POINT('Ctrl Pts',(22.439008584219,55.8431017310511,60.4937922449179)) ;
#7847 = CARTESIAN_POINT('Ctrl Pts',(22.4294962141314,55.8271830724926,60.4950766333802)) ;
#7848 = CARTESIAN_POINT('Ctrl Pts',(22.419986547504,55.8112643008984,60.4963785252368)) ;
#7849 = CARTESIAN_POINT('Ctrl Pts',(22.267917029518,55.5567064895583,60.5171971380081)) ;
#7850 = CARTESIAN_POINT('Ctrl Pts',(22.1164649280643,55.3019957844117,60.5425026636)) ;
#7851 = CARTESIAN_POINT('Ctrl Pts',(21.9656675704896,55.0471908391173,60.5723059396156)) ;
#7852 = CARTESIAN_POINT('Ctrl Pts',(21.9581562962121,55.034498906963,60.5737904522365)) ;
#7853 = CARTESIAN_POINT('Ctrl Pts',(21.9506466823413,55.0218058655745,60.5752861659703)) ;
#7854 = CARTESIAN_POINT('Ctrl Pts',(21.9431388263387,55.0091118266697,60.5767930566487)) ;
#7855 = CARTESIAN_POINT('Ctrl Pts',(21.7904748859319,54.7509925981975,60.6074340104226)) ;
#7856 = CARTESIAN_POINT('Ctrl Pts',(21.6386230866642,54.4926055130901,60.6426783253807)) ;
#7857 = CARTESIAN_POINT('Ctrl Pts',(21.4882181064184,54.2345762733044,60.6823628358805)) ;
#7858 = CARTESIAN_POINT('Ctrl Pts',(21.482727917163,54.2251575070006,60.6838114280269)) ;
#7859 = CARTESIAN_POINT('Ctrl Pts',(21.4772392198183,54.2157389752756,60.6852660449337)) ;
#7860 = CARTESIAN_POINT('Ctrl Pts',(21.4717520252972,54.2063206495464,60.6867266832642)) ;
#7861 = CARTESIAN_POINT('Ctrl Pts',(21.3195365964412,53.9450551732692,60.7272449643323)) ;
#7862 = CARTESIAN_POINT('Ctrl Pts',(21.1685419560353,53.6840579939663,60.7723810594839)) ;
#7863 = CARTESIAN_POINT('Ctrl Pts',(21.019187288141,53.4230444575823,60.8219988105976)) ;
#7864 = CARTESIAN_POINT('Ctrl Pts',(21.0156601431058,53.4168803877747,60.8231705784906)) ;
#7865 = CARTESIAN_POINT('Ctrl Pts',(21.0121339251964,53.4107163826998,60.8243448352793)) ;
#7866 = CARTESIAN_POINT('Ctrl Pts',(21.0086086348855,53.4045524432161,60.8255215807517)) ;
#7867 = CARTESIAN_POINT('Ctrl Pts',(20.8574656807716,53.1402803009587,60.8759732517481)) ;
#7868 = CARTESIAN_POINT('Ctrl Pts',(20.7079846408797,52.8760533725429,60.9310137169923)) ;
#7869 = CARTESIAN_POINT('Ctrl Pts',(20.560170696436,52.6118787196957,60.9906452371905)) ;
#7870 = CARTESIAN_POINT('Ctrl Pts',(20.4091128753672,52.3419065760602,61.0515854112862)) ;
#7871 = CARTESIAN_POINT('Ctrl Pts',(20.2598865368533,52.0715787920577,61.1172958715969)) ;
#7872 = CARTESIAN_POINT('Ctrl Pts',(20.112834022644,51.8011908422988,61.1876330862895)) ;
#7873 = CARTESIAN_POINT('Ctrl Pts',(20.1126494080365,51.8008513882915,61.1877213899636)) ;
#7874 = CARTESIAN_POINT('Ctrl Pts',(20.1124647968594,51.8005119341975,61.1878097009275)) ;
#7875 = CARTESIAN_POINT('Ctrl Pts',(20.1122801891135,51.8001724800175,61.187898019181)) ;
#7876 = CARTESIAN_POINT('Ctrl Pts',(19.9669966220693,51.5330270582816,61.2574031791369)) ;
#7877 = CARTESIAN_POINT('Ctrl Pts',(19.8235382680195,51.265585354454,61.3315844205049)) ;
#7878 = CARTESIAN_POINT('Ctrl Pts',(19.6828053819963,50.998401550286,61.4099799616795)) ;
#7879 = CARTESIAN_POINT('Ctrl Pts',(19.6809136341175,50.9948100344075,61.4110337636935)) ;
#7880 = CARTESIAN_POINT('Ctrl Pts',(19.6790223692999,50.9912185474961,61.4120883321757)) ;
#7881 = CARTESIAN_POINT('Ctrl Pts',(19.6771315896791,50.9876270907846,61.4131436660542)) ;
#7882 = CARTESIAN_POINT('Ctrl Pts',(19.5381827811403,50.7236996475845,61.4906975932342)) ;
#7883 = CARTESIAN_POINT('Ctrl Pts',(19.401773289945,50.4599498020535,61.5724055573758)) ;
#7884 = CARTESIAN_POINT('Ctrl Pts',(19.2679001702012,50.1963788513665,61.6582612121504)) ;
#7885 = CARTESIAN_POINT('Ctrl Pts',(19.2644389106561,50.1895642834336,61.6604809908868)) ;
#7886 = CARTESIAN_POINT('Ctrl Pts',(19.2609794327328,50.1827500045961,61.6627034870573)) ;
#7887 = CARTESIAN_POINT('Ctrl Pts',(19.2575217330171,50.1759360087368,61.6649287021295)) ;
#7888 = CARTESIAN_POINT('Ctrl Pts',(19.1254241611857,49.9156148757619,61.7499405689775)) ;
#7889 = CARTESIAN_POINT('Ctrl Pts',(18.9960431928179,49.6552611188173,61.8388487050089)) ;
#7890 = CARTESIAN_POINT('Ctrl Pts',(18.8694140211807,49.3948957256021,61.9316092105309)) ;
#7891 = CARTESIAN_POINT('Ctrl Pts',(18.8645077978792,49.3848079176935,61.9352031987705)) ;
#7892 = CARTESIAN_POINT('Ctrl Pts',(18.8596058151151,49.3747203101763,61.9388028976143)) ;
#7893 = CARTESIAN_POINT('Ctrl Pts',(18.8547080857952,49.3646329259558,61.9424082972234)) ;
#7894 = CARTESIAN_POINT('Ctrl Pts',(18.7298870483059,49.1075509841603,62.0342936772381)) ;
#7895 = CARTESIAN_POINT('Ctrl Pts',(18.6076690784898,48.8504690628021,62.1300084731121)) ;
#7896 = CARTESIAN_POINT('Ctrl Pts',(18.4884327105145,48.5931578990172,62.229271765735)) ;
#7897 = CARTESIAN_POINT('Ctrl Pts',(18.4822469141894,48.5798089981879,62.234421390142)) ;
#7898 = CARTESIAN_POINT('Ctrl Pts',(18.4760689516882,48.5664590689812,62.2395807235543)) ;
#7899 = CARTESIAN_POINT('Ctrl Pts',(18.4698988891753,48.5531081058639,62.2447497176984)) ;
#7900 = CARTESIAN_POINT('Ctrl Pts',(18.3524691682294,48.2990102146422,62.3431269284067)) ;
#7901 = CARTESIAN_POINT('Ctrl Pts',(18.2378210041666,48.0446012919297,62.4450654543122)) ;
#7902 = CARTESIAN_POINT('Ctrl Pts',(18.1262517854023,47.7903648312084,62.550326771146)) ;
#7903 = CARTESIAN_POINT('Ctrl Pts',(18.1189739283107,47.7737805380753,62.5571931526595)) ;
#7904 = CARTESIAN_POINT('Ctrl Pts',(18.11170890229,47.7571963611373,62.5640739293288)) ;
#7905 = CARTESIAN_POINT('Ctrl Pts',(18.104456753659,47.7406123516807,62.5709690693567)) ;
#7906 = CARTESIAN_POINT('Ctrl Pts',(17.9946923640913,47.4896062337403,62.6753299801235)) ;
#7907 = CARTESIAN_POINT('Ctrl Pts',(17.8881599074056,47.2387261489802,62.7826999639579)) ;
#7908 = CARTESIAN_POINT('Ctrl Pts',(17.7848097317844,46.9878897404752,62.893100191579)) ;
#7909 = CARTESIAN_POINT('Ctrl Pts',(17.7766757639826,46.9681481652137,62.9017890195504)) ;
#7910 = CARTESIAN_POINT('Ctrl Pts',(17.7685617599153,46.9484074501541,62.9104963668765)) ;
#7911 = CARTESIAN_POINT('Ctrl Pts',(17.7604677083785,46.9286675886393,62.9192222283657)) ;
#7912 = CARTESIAN_POINT('Ctrl Pts',(17.6589239088363,46.6810214584483,63.0286923899853)) ;
#7913 = CARTESIAN_POINT('Ctrl Pts',(17.5604595377658,46.4334531760664,63.1411577287807)) ;
#7914 = CARTESIAN_POINT('Ctrl Pts',(17.4653464547407,46.1857600468477,63.256308049298)) ;
#7915 = CARTESIAN_POINT('Ctrl Pts',(17.4566036038392,46.162991947768,63.2668927349324)) ;
#7916 = CARTESIAN_POINT('Ctrl Pts',(17.4478888840466,46.1402223084084,63.277500332783)) ;
#7917 = CARTESIAN_POINT('Ctrl Pts',(17.4392025259141,46.1174510138862,63.288130583901)) ;
#7918 = CARTESIAN_POINT('Ctrl Pts',(17.3458579122278,45.8727480373453,63.4023644974539)) ;
#7919 = CARTESIAN_POINT('Ctrl Pts',(17.2557287797025,45.627974343213,63.5192728483348)) ;
#7920 = CARTESIAN_POINT('Ctrl Pts',(17.1688739128827,45.3830610445956,63.6388169494918)) ;
#7921 = CARTESIAN_POINT('',(1.06650400490287,48.5844537758935,41.3386313446643)) ;
#7922 = CARTESIAN_POINT('Ctrl Pts',(0.569856645481657,45.3830586252741,51.5789200251186)) ;
#7923 = CARTESIAN_POINT('Ctrl Pts',(0.205152783399156,45.4231929016304,51.2052420971489)) ;
#7924 = CARTESIAN_POINT('Ctrl Pts',(-0.115007591050823,45.4870033446877,50.7935164752995)) ;
#7925 = CARTESIAN_POINT('Ctrl Pts',(-0.66183104916004,45.6539797372435,49.9030397345301)) ;
#7926 = CARTESIAN_POINT('Ctrl Pts',(-0.884618914799949,45.7573388893142,49.4261784970127)) ;
#7927 = CARTESIAN_POINT('Ctrl Pts',(-1.34560813242504,46.0833507061678,48.0631169416231)) ;
#7928 = CARTESIAN_POINT('Ctrl Pts',(-1.46302722997465,46.3336877227691,47.1527476308917)) ;
#7929 = CARTESIAN_POINT('Ctrl Pts',(-1.34627520533182,46.9107591797132,45.2786955776573)) ;
#7930 = CARTESIAN_POINT('Ctrl Pts',(-1.08232247700463,47.2383195349501,44.3334069001318)) ;
#7931 = CARTESIAN_POINT('Ctrl Pts',(-0.215987177965692,47.9083523080807,42.6567201668803)) ;
#7932 = CARTESIAN_POINT('Ctrl Pts',(0.364376757671241,48.2450338483641,41.9307797259103)) ;
#7933 = CARTESIAN_POINT('Ctrl Pts',(1.06650400490289,48.5844537758935,41.3386313446643)) ;
#7934 = CARTESIAN_POINT('',(1.10488630355745,48.6029307720944,41.3065881552646)) ;
#7935 = CARTESIAN_POINT('Origin',(-21.0084886185846,48.3727968889151,14.7032769090681)) ;
#7936 = CARTESIAN_POINT('',(16.7460459354099,55.0677871747466,33.875818260496)) ;
#7937 = CARTESIAN_POINT('Ctrl Pts',(1.10488630355745,48.6029307720944,41.3065881552646)) ;
#7938 = CARTESIAN_POINT('Ctrl Pts',(1.48456672001327,48.785356686239,40.9910857258634)) ;
#7939 = CARTESIAN_POINT('Ctrl Pts',(1.872950270617,48.9676174488035,40.6863609088291)) ;
#7940 = CARTESIAN_POINT('Ctrl Pts',(3.14601974869293,49.5650439193917,39.6875136013786)) ;
#7941 = CARTESIAN_POINT('Ctrl Pts',(4.50582053922401,50.16247038998,38.8103912326747)) ;
#7942 = CARTESIAN_POINT('Ctrl Pts',(5.86562132975509,50.7598968605682,37.9332688639709)) ;
#7943 = CARTESIAN_POINT('Ctrl Pts',(7.30055209184877,51.3573233311564,37.1853547327988)) ;
#7944 = CARTESIAN_POINT('Ctrl Pts',(8.73548285394244,51.9547498017447,36.4374406016267)) ;
#7945 = CARTESIAN_POINT('Ctrl Pts',(10.2333012642789,52.5521762723329,35.8251156476465)) ;
#7946 = CARTESIAN_POINT('Ctrl Pts',(11.7311196746153,53.1496027429211,35.2127906936662)) ;
#7947 = CARTESIAN_POINT('Ctrl Pts',(13.2790468746333,53.7470292135094,34.7412790574855)) ;
#7948 = CARTESIAN_POINT('Ctrl Pts',(14.8269740746514,54.3444556840976,34.2697674213048)) ;
#7949 = CARTESIAN_POINT('Ctrl Pts',(16.4118036952644,54.9418821546858,33.9430918739531)) ;
#7950 = CARTESIAN_POINT('Ctrl Pts',(16.5787680203067,55.0048219850164,33.9086760846708)) ;
#7951 = CARTESIAN_POINT('Ctrl Pts',(16.7460459354099,55.0677871747466,33.875818260496)) ;
#7952 = CARTESIAN_POINT('',(16.7951325976017,55.0862551252693,33.8663068761758)) ;
#7953 = CARTESIAN_POINT('Origin',(9.80672900050722,55.553531622349,-1.52672131664897)) ;
#7954 = CARTESIAN_POINT('Ctrl Pts',(16.7951325976017,55.0862551252692,33.8663068761758)) ;
#7955 = CARTESIAN_POINT('Ctrl Pts',(17.3269366349108,55.2861476150253,33.7660169109597)) ;
#7956 = CARTESIAN_POINT('Ctrl Pts',(17.8689949355364,55.4856143511659,33.7276579994428)) ;
#7957 = CARTESIAN_POINT('Ctrl Pts',(18.9906738261853,55.8948726679075,33.7786821697219)) ;
#7958 = CARTESIAN_POINT('Ctrl Pts',(19.5668322091791,56.1030296514258,33.8772515792835)) ;
#7959 = CARTESIAN_POINT('Ctrl Pts',(21.042556999384,56.639522788727,34.3251774027028)) ;
#7960 = CARTESIAN_POINT('Ctrl Pts',(21.8999253408597,56.9553075668519,34.791153792355)) ;
#7961 = CARTESIAN_POINT('Ctrl Pts',(23.3209771338725,57.5027527547765,36.0053548133869)) ;
#7962 = CARTESIAN_POINT('Ctrl Pts',(23.8915820353075,57.7356391827932,36.71956623351)) ;
#7963 = CARTESIAN_POINT('Ctrl Pts',(24.6195664683639,58.058368696673,38.1284250825275)) ;
#7964 = CARTESIAN_POINT('Ctrl Pts',(24.8427619123796,58.167950706673,38.7711976908919)) ;
#7965 = CARTESIAN_POINT('Ctrl Pts',(25.0783873637464,58.3023924852745,40.0133620327521)) ;
#7966 = CARTESIAN_POINT('Ctrl Pts',(25.1153550438448,58.3364158759195,40.5995114251688)) ;
#7967 = CARTESIAN_POINT('Ctrl Pts',(25.0785449650548,58.3353824278239,41.1845908766823)) ;
#7968 = CARTESIAN_POINT('Ctrl Pts',(-4.89668542317829,45.3830585852922,47.7308516627133)) ;
#7969 = CARTESIAN_POINT('Ctrl Pts',(-3.94930237640841,45.9804850758286,46.4190251645259)) ;
#7970 = CARTESIAN_POINT('Ctrl Pts',(-2.88492061603778,46.5779115664506,45.2002081697134)) ;
#7971 = CARTESIAN_POINT('Ctrl Pts',(-1.82053889135939,47.1753380370388,43.9813912157718)) ;
#7972 = CARTESIAN_POINT('Ctrl Pts',(-0.64823939064702,47.772764507627,42.8659822756631)) ;
#7973 = CARTESIAN_POINT('Ctrl Pts',(0.524060110065356,48.3701909782152,41.7505733355544)) ;
#7974 = CARTESIAN_POINT('Ctrl Pts',(1.7942757408128,48.9676174488035,40.7480886850736)) ;
#7975 = CARTESIAN_POINT('Ctrl Pts',(3.06449137156023,49.5650439193917,39.7456040345928)) ;
#7976 = CARTESIAN_POINT('Ctrl Pts',(4.42178610044663,50.16247038998,38.8645965193115)) ;
#7977 = CARTESIAN_POINT('Ctrl Pts',(5.77908082933302,50.7598968605682,37.9835890040303)) ;
#7978 = CARTESIAN_POINT('Ctrl Pts',(7.21187469630014,51.3573233311564,37.2315750694345)) ;
#7979 = CARTESIAN_POINT('Ctrl Pts',(8.64466856326726,51.9547498017447,36.4795611348387)) ;
#7980 = CARTESIAN_POINT('Ctrl Pts',(10.140737476231,52.5521762723329,35.8629566986657)) ;
#7981 = CARTESIAN_POINT('Ctrl Pts',(11.6368063891948,53.1496027429212,35.2463522624928)) ;
#7982 = CARTESIAN_POINT('Ctrl Pts',(13.1833864156889,53.7470292135094,34.7704179763834)) ;
#7983 = CARTESIAN_POINT('Ctrl Pts',(14.729966442183,54.3444556840976,34.2944836902741)) ;
#7984 = CARTESIAN_POINT('Ctrl Pts',(16.31386270673,54.9418821546858,33.9632800577477)) ;
#7985 = CARTESIAN_POINT('Ctrl Pts',(17.8977589712771,55.5393086252741,33.6320764252214)) ;
#7986 = CARTESIAN_POINT('Ctrl Pts',(19.5054582294142,56.1367350958623,33.4484291588917)) ;
#7987 = CARTESIAN_POINT('Ctrl Pts',(21.1131574875512,56.7341615664506,33.2647818925619)) ;
#7988 = CARTESIAN_POINT('Ctrl Pts',(22.7309434160666,57.3315880370388,33.230257806153)) ;
#7989 = CARTESIAN_POINT('Ctrl Pts',(24.1543552347212,57.8572347768351,33.199881727491)) ;
#7990 = CARTESIAN_POINT('Ctrl Pts',(25.5755313903897,58.3831186720347,33.2852178054411)) ;
#7991 = CARTESIAN_POINT('Ctrl Pts',(17.351282019329,45.3830585852922,63.8949460662004)) ;
#7992 = CARTESIAN_POINT('Ctrl Pts',(17.5513538557446,45.9804850758286,63.6117052136026)) ;
#7993 = CARTESIAN_POINT('Ctrl Pts',(17.7767063905955,46.5779115664506,63.3481329173662)) ;
#7994 = CARTESIAN_POINT('Ctrl Pts',(18.0020589178895,47.1753380370388,63.0845606299682)) ;
#7995 = CARTESIAN_POINT('Ctrl Pts',(18.2507695135888,47.772764507627,62.8429056034762)) ;
#7996 = CARTESIAN_POINT('Ctrl Pts',(18.4994801092881,48.3701909782152,62.6012505769841)) ;
#7997 = CARTESIAN_POINT('Ctrl Pts',(18.7694268622831,48.9676174488035,62.3835745268788)) ;
#7998 = CARTESIAN_POINT('Ctrl Pts',(19.0393736152781,49.5650439193917,62.1658984767735)) ;
#7999 = CARTESIAN_POINT('Ctrl Pts',(19.3282534350527,50.16247038998,61.974058538364)) ;
#8000 = CARTESIAN_POINT('Ctrl Pts',(19.6171332548274,50.7598968605682,61.7822185999545)) ;
#8001 = CARTESIAN_POINT('Ctrl Pts',(19.9224815206155,51.3573233311564,61.6178514839545)) ;
#8002 = CARTESIAN_POINT('Ctrl Pts',(20.2278297864037,51.9547498017447,61.4534843679545)) ;
#8003 = CARTESIAN_POINT('Ctrl Pts',(20.5470413744644,52.5521762723329,61.3179923966435)) ;
#8004 = CARTESIAN_POINT('Ctrl Pts',(20.8662529625251,53.1496027429211,61.1825004253324)) ;
#8005 = CARTESIAN_POINT('Ctrl Pts',(21.1966044721399,53.7470292135094,61.0770395684365)) ;
#8006 = CARTESIAN_POINT('Ctrl Pts',(21.5269559817547,54.3444556840976,60.9715787115406)) ;
#8007 = CARTESIAN_POINT('Ctrl Pts',(21.8656289703221,54.9418821546858,60.8970487239063)) ;
#8008 = CARTESIAN_POINT('Ctrl Pts',(22.2043019588896,55.5393086252741,60.8225187362721)) ;
#8009 = CARTESIAN_POINT('Ctrl Pts',(22.5484069878841,56.1367350958623,60.7795554814755)) ;
#8010 = CARTESIAN_POINT('Ctrl Pts',(22.8925120168785,56.7341615664506,60.7365922266788)) ;
#8011 = CARTESIAN_POINT('Ctrl Pts',(23.2391133035206,57.3315880370388,60.7255622520614)) ;
#8012 = CARTESIAN_POINT('Ctrl Pts',(23.5440710603357,57.8572347768351,60.7158575093304)) ;
#8013 = CARTESIAN_POINT('Ctrl Pts',(23.8488094920358,58.3831186720347,60.7309539896547)) ;
#8014 = CARTESIAN_POINT('',(23.8673496931823,58.3830537363176,60.4362583055437)) ;
#8015 = CARTESIAN_POINT('Ctrl Pts',(17.1123854551458,45.3830674541108,63.721395608331)) ;
#8016 = CARTESIAN_POINT('Ctrl Pts',(17.1182555903267,45.3999249614348,63.7130941959663)) ;
#8017 = CARTESIAN_POINT('Ctrl Pts',(17.1242245528045,45.4170195560983,63.7046879792065)) ;
#8018 = CARTESIAN_POINT('Ctrl Pts',(17.136110401805,45.4509660823352,63.6880190307945)) ;
#8019 = CARTESIAN_POINT('Ctrl Pts',(17.1420688908599,45.4679374856688,63.6796974657324)) ;
#8020 = CARTESIAN_POINT('Ctrl Pts',(17.1599909175645,45.5188462146264,63.6547715850251)) ;
#8021 = CARTESIAN_POINT('Ctrl Pts',(17.1720010144541,45.5527780591985,63.6382060836503)) ;
#8022 = CARTESIAN_POINT('Ctrl Pts',(17.2082164796663,45.6545524513439,63.5886655433169)) ;
#8023 = CARTESIAN_POINT('Ctrl Pts',(17.2326070347849,45.7223738576063,63.5558464774858)) ;
#8024 = CARTESIAN_POINT('Ctrl Pts',(17.2882647437757,45.8755455989769,63.4821716097248)) ;
#8025 = CARTESIAN_POINT('Ctrl Pts',(17.3196760141081,45.9608834226833,63.4414374945538)) ;
#8026 = CARTESIAN_POINT('Ctrl Pts',(17.370165521914,46.0963466756243,63.3772837588605)) ;
#8027 = CARTESIAN_POINT('Ctrl Pts',(17.3889996936742,46.1464973799216,63.3536369427366)) ;
#8028 = CARTESIAN_POINT('Ctrl Pts',(17.4955782697342,46.4282028809689,63.2214096186718)) ;
#8029 = CARTESIAN_POINT('Ctrl Pts',(17.5860373897972,46.6594344485538,63.1151569797222)) ;
#8030 = CARTESIAN_POINT('Ctrl Pts',(17.6949271722414,46.9296827699032,62.9939899321235)) ;
#8031 = CARTESIAN_POINT('Ctrl Pts',(17.7107643919321,46.9687950424163,62.976526950364)) ;
#8032 = CARTESIAN_POINT('Ctrl Pts',(17.8251792031112,47.2499758749393,62.8515103176276)) ;
#8033 = CARTESIAN_POINT('Ctrl Pts',(17.9265852618937,47.4918541916698,62.746770719906)) ;
#8034 = CARTESIAN_POINT('Ctrl Pts',(18.1520599948226,48.0143150857794,62.526576356011)) ;
#8035 = CARTESIAN_POINT('Ctrl Pts',(18.2770523113096,48.2952954282315,62.4122348405312)) ;
#8036 = CARTESIAN_POINT('Ctrl Pts',(18.4133728607043,48.593120430708,62.2954439777444)) ;
#8037 = CARTESIAN_POINT('Ctrl Pts',(18.4211678305597,48.6101204742723,62.2887923752948)) ;
#8038 = CARTESIAN_POINT('Ctrl Pts',(18.5501994677138,48.8910362150329,62.1791264958796)) ;
#8039 = CARTESIAN_POINT('Ctrl Pts',(18.6746809217014,49.154922679681,62.0797249566039)) ;
#8040 = CARTESIAN_POINT('Ctrl Pts',(18.8049007382563,49.4249376060055,61.9821239583166)) ;
#8041 = CARTESIAN_POINT('Ctrl Pts',(18.8077299832015,49.4308011237539,61.980006410541)) ;
#8042 = CARTESIAN_POINT('Ctrl Pts',(18.9409149634897,49.7066812295575,61.8804651685687)) ;
#8043 = CARTESIAN_POINT('Ctrl Pts',(19.0744281513532,49.9768666464288,61.7870358280021)) ;
#8044 = CARTESIAN_POINT('Ctrl Pts',(19.2136570314282,50.2527043291671,61.6959902898179)) ;
#8045 = CARTESIAN_POINT('Ctrl Pts',(19.2163616978931,50.2580605419638,61.6942240338067)) ;
#8046 = CARTESIAN_POINT('Ctrl Pts',(19.3530104917543,50.5285623062289,61.6051079770347)) ;
#8047 = CARTESIAN_POINT('Ctrl Pts',(19.4896723531249,50.7940892820341,61.5218500905069)) ;
#8048 = CARTESIAN_POINT('Ctrl Pts',(19.6378635331462,51.0767673302897,61.4377267779672)) ;
#8049 = CARTESIAN_POINT('Ctrl Pts',(19.6466506236689,51.0935097128495,61.4327611474076)) ;
#8050 = CARTESIAN_POINT('Ctrl Pts',(19.7297354246784,51.2516332986689,61.3860219320458)) ;
#8051 = CARTESIAN_POINT('Ctrl Pts',(19.8048581245304,51.3931664825954,61.3453693189635)) ;
#8052 = CARTESIAN_POINT('Ctrl Pts',(19.9411643864943,51.6479675595812,61.2744794803297)) ;
#8053 = CARTESIAN_POINT('Ctrl Pts',(20.0021436698153,51.7612319406867,61.2437773525758)) ;
#8054 = CARTESIAN_POINT('Ctrl Pts',(20.0787570680475,51.9026374456283,61.2064554735793)) ;
#8055 = CARTESIAN_POINT('Ctrl Pts',(20.0940444369611,51.9308091085123,61.1990699995767)) ;
#8056 = CARTESIAN_POINT('Ctrl Pts',(20.2630277485757,52.2417252333154,61.1181119533642)) ;
#8057 = CARTESIAN_POINT('Ctrl Pts',(20.4190788234136,52.524119549279,61.0495454272598)) ;
#8058 = CARTESIAN_POINT('Ctrl Pts',(20.7067517642157,53.0381974993202,60.9342400965987)) ;
#8059 = CARTESIAN_POINT('Ctrl Pts',(20.8376177185125,53.2697333986823,60.8858199040384)) ;
#8060 = CARTESIAN_POINT('Ctrl Pts',(20.9988733465646,53.5522259966914,60.831031906915)) ;
#8061 = CARTESIAN_POINT('Ctrl Pts',(21.0280209326871,53.6031771340238,60.8213204978166)) ;
#8062 = CARTESIAN_POINT('Ctrl Pts',(21.183426574497,53.8742457620983,60.7705601480465)) ;
#8063 = CARTESIAN_POINT('Ctrl Pts',(21.3107285320407,54.0945463050598,60.7325518486177)) ;
#8064 = CARTESIAN_POINT('Ctrl Pts',(21.4752926476314,54.3774106831902,60.6879647640456)) ;
#8065 = CARTESIAN_POINT('Ctrl Pts',(21.5117056194114,54.4398806254182,60.6783814028631)) ;
#8066 = CARTESIAN_POINT('Ctrl Pts',(21.6702778897318,54.7114321393038,60.6378739818295)) ;
#8067 = CARTESIAN_POINT('Ctrl Pts',(21.7932788702932,54.9205828276702,60.6096170503781)) ;
#8068 = CARTESIAN_POINT('Ctrl Pts',(21.9603429329453,55.203368432955,60.5754722779609)) ;
#8069 = CARTESIAN_POINT('Ctrl Pts',(22.0040512805472,55.2772338818095,60.5669287745172)) ;
#8070 = CARTESIAN_POINT('Ctrl Pts',(22.1647806110715,55.5485088102251,60.5369417955332)) ;
#8071 = CARTESIAN_POINT('Ctrl Pts',(22.2821573285742,55.7457837763586,60.5178093132553)) ;
#8072 = CARTESIAN_POINT('Ctrl Pts',(22.450831654825,56.0282588904741,60.4942633908894)) ;
#8073 = CARTESIAN_POINT('Ctrl Pts',(22.5018036784155,56.1134884206088,60.4876618904377)) ;
#8074 = CARTESIAN_POINT('Ctrl Pts',(22.6640819348038,56.3844426291133,60.4682748073054)) ;
#8075 = CARTESIAN_POINT('Ctrl Pts',(22.7754796800465,56.5701302611216,60.4573949544576)) ;
#8076 = CARTESIAN_POINT('Ctrl Pts',(22.9452620536937,56.8526653483,60.4444955791702)) ;
#8077 = CARTESIAN_POINT('Ctrl Pts',(23.0034860747583,56.9494716030797,60.4407289267428)) ;
#8078 = CARTESIAN_POINT('Ctrl Pts',(23.1666024780397,57.2204413601139,60.4320127348201)) ;
#8079 = CARTESIAN_POINT('Ctrl Pts',(23.2716417516358,57.3946576755336,60.4285278227131)) ;
#8080 = CARTESIAN_POINT('Ctrl Pts',(23.4421351823808,57.6774250653637,60.426319247965)) ;
#8081 = CARTESIAN_POINT('Ctrl Pts',(23.5075650498815,57.7859396412674,60.4262949212388)) ;
#8082 = CARTESIAN_POINT('Ctrl Pts',(23.5893294576124,57.921622741885,60.4272945872543)) ;
#8083 = CARTESIAN_POINT('Ctrl Pts',(23.6056644130462,57.9487278912592,60.4275457298318)) ;
#8084 = CARTESIAN_POINT('Ctrl Pts',(23.662889166053,58.0436810159816,60.4286055603454)) ;
#8085 = CARTESIAN_POINT('Ctrl Pts',(23.7037872596467,58.1115399743061,60.4296853156621)) ;
#8086 = CARTESIAN_POINT('Ctrl Pts',(23.7651325370338,58.2133484522833,60.4317881034382)) ;
#8087 = CARTESIAN_POINT('Ctrl Pts',(23.785578913315,58.2472850649071,60.4325694758602)) ;
#8088 = CARTESIAN_POINT('Ctrl Pts',(23.8162473293565,58.2981973836593,60.4338623341475)) ;
#8089 = CARTESIAN_POINT('Ctrl Pts',(23.8264699432712,58.3151693899118,60.4343134204592)) ;
#8090 = CARTESIAN_POINT('Ctrl Pts',(23.8394771596519,58.3367668565656,60.4349130214635)) ;
#8091 = CARTESIAN_POINT('Ctrl Pts',(23.8422673657082,58.3413999128699,60.4350431404392)) ;
#8092 = CARTESIAN_POINT('Ctrl Pts',(23.8525116996386,58.3584108602029,60.4355263988823)) ;
#8093 = CARTESIAN_POINT('Ctrl Pts',(23.8599705749502,58.3707975233386,60.4358890556515)) ;
#8094 = CARTESIAN_POINT('Ctrl Pts',(23.8673485046708,58.3830508753326,60.436258249004)) ;
#8095 = CARTESIAN_POINT('',(25.0785449650548,58.3831162793798,41.1845908766823)) ;
#8096 = CARTESIAN_POINT('Ctrl Pts',(23.8673327885118,58.38309009802,60.4362572466387)) ;
#8097 = CARTESIAN_POINT('Ctrl Pts',(24.0692014846605,58.3831052593851,57.2276461840538)) ;
#8098 = CARTESIAN_POINT('Ctrl Pts',(24.2710701808123,58.3831073991803,54.0190351214176)) ;
#8099 = CARTESIAN_POINT('Ctrl Pts',(24.6748075729936,58.3831134572106,47.6018129980939)) ;
#8100 = CARTESIAN_POINT('Ctrl Pts',(24.8766762690243,58.383115023513,44.393201937388)) ;
#8101 = CARTESIAN_POINT('Ctrl Pts',(25.0785449650548,58.3831162793798,41.1845908766823)) ;
#8102 = CARTESIAN_POINT('',(16.7460321974209,55.1047242171091,33.8757481656485)) ;
#8103 = CARTESIAN_POINT('Ctrl Pts',(25.0785449650548,58.3831162793797,41.1845908766823)) ;
#8104 = CARTESIAN_POINT('Ctrl Pts',(25.1155757155261,58.3831165097557,40.5960039492146)) ;
#8105 = CARTESIAN_POINT('Ctrl Pts',(25.0779368416003,58.3477204189414,40.0063991848858)) ;
#8106 = CARTESIAN_POINT('Ctrl Pts',(24.838960064421,58.2097833704152,38.7566097094888)) ;
#8107 = CARTESIAN_POINT('Ctrl Pts',(24.6125958308685,58.0979491851445,38.1099399214988)) ;
#8108 = CARTESIAN_POINT('Ctrl Pts',(23.8774133952963,57.7707078254696,36.6991149643586)) ;
#8109 = CARTESIAN_POINT('Ctrl Pts',(23.303921871022,57.5360202457533,35.9865255376264)) ;
#8110 = CARTESIAN_POINT('Ctrl Pts',(21.8778342174311,56.9856758817169,34.7770271162412)) ;
#8111 = CARTESIAN_POINT('Ctrl Pts',(21.0183674292568,56.6687344805944,34.3140462118494)) ;
#8112 = CARTESIAN_POINT('Ctrl Pts',(19.5365000825384,56.1294192803768,33.8704549815538)) ;
#8113 = CARTESIAN_POINT('Ctrl Pts',(18.9557023901162,55.9194276565173,33.77390896011)) ;
#8114 = CARTESIAN_POINT('Ctrl Pts',(17.8260154983585,55.506862709361,33.7288845369499)) ;
#8115 = CARTESIAN_POINT('Ctrl Pts',(17.2806296106359,55.3059551814418,33.77097165732)) ;
#8116 = CARTESIAN_POINT('Ctrl Pts',(16.7460321974209,55.104724217109,33.8757481656485)) ;
#8117 = CARTESIAN_POINT('',(1.10484064496481,48.6398835186857,41.3065332251917)) ;
#8118 = CARTESIAN_POINT('Ctrl Pts',(1.10484064496481,48.6398835186857,41.3065332251917)) ;
#8119 = CARTESIAN_POINT('Ctrl Pts',(1.44601886987501,48.8038201453524,41.0229414372091)) ;
#8120 = CARTESIAN_POINT('Ctrl Pts',(1.79427577681365,48.9676174488035,40.7480887309581)) ;
#8121 = CARTESIAN_POINT('Ctrl Pts',(3.06449140543972,49.5650439193917,39.7456040821417)) ;
#8122 = CARTESIAN_POINT('Ctrl Pts',(4.42178613206022,50.16247038998,38.864596568322)) ;
#8123 = CARTESIAN_POINT('Ctrl Pts',(5.77908085868072,50.7598968605682,37.9835890545023)) ;
#8124 = CARTESIAN_POINT('Ctrl Pts',(7.21187472325676,51.3573233311564,37.2315751211528)) ;
#8125 = CARTESIAN_POINT('Ctrl Pts',(8.6446685878328,51.9547498017447,36.4795611878033)) ;
#8126 = CARTESIAN_POINT('Ctrl Pts',(10.1407374983007,52.5521762723329,35.8629567526507)) ;
#8127 = CARTESIAN_POINT('Ctrl Pts',(11.6368064087686,53.1496027429211,35.2463523174981)) ;
#8128 = CARTESIAN_POINT('Ctrl Pts',(13.1833864326833,53.7470292135094,34.7704180321744)) ;
#8129 = CARTESIAN_POINT('Ctrl Pts',(14.729966456598,54.3444556840976,34.2944837468508)) ;
#8130 = CARTESIAN_POINT('Ctrl Pts',(16.3138627185042,54.9418821546858,33.9632801148688)) ;
#8131 = CARTESIAN_POINT('Ctrl Pts',(16.5296717625019,55.0232827101246,33.9181529554041)) ;
#8132 = CARTESIAN_POINT('Ctrl Pts',(16.7460321974209,55.1047242171091,33.8757481656485)) ;
#8133 = CARTESIAN_POINT('Ctrl Pts',(1.10484064496482,48.6398835186857,41.3065332251917)) ;
#8134 = CARTESIAN_POINT('Ctrl Pts',(0.688510729437327,48.4398363968332,41.6525920780571)) ;
#8135 = CARTESIAN_POINT('Ctrl Pts',(0.313395234053494,48.2402511072957,42.0460608191272)) ;
#8136 = CARTESIAN_POINT('Ctrl Pts',(-0.361789782441167,47.8311034847342,42.9428152265227)) ;
#8137 = CARTESIAN_POINT('Ctrl Pts',(-0.652682875411226,47.62311970224,43.4491246060191)) ;
#8138 = CARTESIAN_POINT('Ctrl Pts',(-1.24789105437135,47.0862681322599,44.8711986217157)) ;
#8139 = CARTESIAN_POINT('Ctrl Pts',(-1.43533510647897,46.770327077101,45.8290078005203)) ;
#8140 = CARTESIAN_POINT('Ctrl Pts',(-1.4052997838034,46.2216257312613,47.6989976412504)) ;
#8141 = CARTESIAN_POINT('Ctrl Pts',(-1.21835231594779,45.9879058539332,48.5942607190196)) ;
#8142 = CARTESIAN_POINT('Ctrl Pts',(-0.596411936332433,45.6640068779433,50.0526247730249)) ;
#8143 = CARTESIAN_POINT('Ctrl Pts',(-0.243839452258383,45.5539383973837,50.6333814528433)) ;
#8144 = CARTESIAN_POINT('Ctrl Pts',(0.562423093908943,45.4179657782124,51.605995305929)) ;
#8145 = CARTESIAN_POINT('Ctrl Pts',(0.990533295549593,45.3830586252741,52.0081662996818)) ;
#8146 = CARTESIAN_POINT('Ctrl Pts',(1.46489508963947,45.3830586252741,52.352810316749)) ;
#8147 = CARTESIAN_POINT('Origin',(5.57939185568678,45.3822493559848,46.6896913561244)) ;
#8148 = CARTESIAN_POINT('',(1.10484064496481,45.3822493559848,41.3065332251917)) ;
#8149 = CARTESIAN_POINT('Origin',(23.4776880157599,45.3822493559848,68.2224337400009)) ;
#8150 = CARTESIAN_POINT('',(16.7460321974209,45.3822493559848,33.8757481656485)) ;
#8151 = CARTESIAN_POINT('Origin',(18.0923578658931,45.3822493559848,40.74505724258)) ;
#8152 = CARTESIAN_POINT('',(25.0785449650548,45.3822493559848,41.1845908766823)) ;
#8153 = CARTESIAN_POINT('Origin',(23.8487920953129,45.3822493559848,60.7309531278765)) ;
#8154 = CARTESIAN_POINT('Ctrl Pts',(23.8550298361323,57.8271591833517,60.6318070761082)) ;
#8155 = CARTESIAN_POINT('Ctrl Pts',(23.8550352275545,57.8726762313018,60.6317213819064)) ;
#8156 = CARTESIAN_POINT('Ctrl Pts',(23.855296076976,57.918955920172,60.627575298638)) ;
#8157 = CARTESIAN_POINT('Ctrl Pts',(23.8563587264365,58.0070760893886,60.6106849690344)) ;
#8158 = CARTESIAN_POINT('Ctrl Pts',(23.8571732808255,58.0511720064474,60.59773799811)) ;
#8159 = CARTESIAN_POINT('Ctrl Pts',(23.8594428410483,58.1280396084341,60.5616643711575)) ;
#8160 = CARTESIAN_POINT('Ctrl Pts',(23.8607537844068,58.1581206858333,60.5408275229561)) ;
#8161 = CARTESIAN_POINT('Ctrl Pts',(23.8630017351916,58.1912258389784,60.5050973681879)) ;
#8162 = CARTESIAN_POINT('Ctrl Pts',(23.8638861728135,58.2011509267549,60.4910396347398)) ;
#8163 = CARTESIAN_POINT('Ctrl Pts',(23.8656938863924,58.2136664809647,60.4623068500248)) ;
#8164 = CARTESIAN_POINT('Ctrl Pts',(23.8665670166679,58.2169696033441,60.4484288416232)) ;
#8165 = CARTESIAN_POINT('Ctrl Pts',(23.8674708869362,58.2172758076353,60.4340622350259)) ;
#8166 = CARTESIAN_POINT('Ctrl Pts',(23.8673327749686,58.3830247512608,60.4362574619018)) ;
#8167 = CARTESIAN_POINT('Ctrl Pts',(23.8668913274621,58.3830247228383,60.4432740691308)) ;
#8168 = CARTESIAN_POINT('Ctrl Pts',(23.8664534737013,58.3837424765051,60.4502335554086)) ;
#8169 = CARTESIAN_POINT('Ctrl Pts',(23.8655593939275,58.3866521090668,60.4644445465522)) ;
#8170 = CARTESIAN_POINT('Ctrl Pts',(23.8651108505696,58.3889169428591,60.4715739391106)) ;
#8171 = CARTESIAN_POINT('Ctrl Pts',(23.8636819932964,58.3985444430715,60.4942849752503)) ;
#8172 = CARTESIAN_POINT('Ctrl Pts',(23.8627851038498,58.408561172042,60.5085406252432)) ;
#8173 = CARTESIAN_POINT('Ctrl Pts',(23.8605808340613,58.4411881110197,60.543576490452)) ;
#8174 = CARTESIAN_POINT('Ctrl Pts',(23.859318365517,58.4701790972424,60.5636428530834)) ;
#8175 = CARTESIAN_POINT('Ctrl Pts',(23.8571082748939,58.5450324120561,60.5987712378107)) ;
#8176 = CARTESIAN_POINT('Ctrl Pts',(23.8563138253378,58.5884045335181,60.6113986531833)) ;
#8177 = CARTESIAN_POINT('Ctrl Pts',(23.8552791568201,58.6752752681888,60.6278442384343)) ;
#8178 = CARTESIAN_POINT('Ctrl Pts',(23.8550297927293,58.7210386855151,60.6318077659803)) ;
#8179 = CARTESIAN_POINT('Ctrl Pts',(23.8550298103818,58.7660385537572,60.6318074854008)) ;
#8180 = CARTESIAN_POINT('Ctrl Pts',(23.9138964394444,58.2943663992286,60.4365240299658)) ;
#8181 = CARTESIAN_POINT('Ctrl Pts',(23.9017702691677,58.2924602039142,60.6324139695376)) ;
#8182 = CARTESIAN_POINT('Ctrl Pts',(24.0693253324374,58.191081348463,60.6454973349943)) ;
#8183 = CARTESIAN_POINT('Ctrl Pts',(23.5875061423568,57.7522999682109,60.4182390850653)) ;
#8184 = CARTESIAN_POINT('Ctrl Pts',(23.5835904522462,57.7503889244903,60.6146349637289)) ;
#8185 = CARTESIAN_POINT('Ctrl Pts',(23.7516792744512,57.6489874076351,60.6206942679821)) ;
#8186 = CARTESIAN_POINT('Ctrl Pts',(23.2604720834133,57.2111033102479,60.4205244415559)) ;
#8187 = CARTESIAN_POINT('Ctrl Pts',(23.2647892639797,57.2091968025947,60.6169122222677)) ;
#8188 = CARTESIAN_POINT('Ctrl Pts',(23.4330242330242,57.1078632090985,60.6159239897169)) ;
#8189 = CARTESIAN_POINT('Ctrl Pts',(22.7725719487901,56.3997926693515,60.4545477382972)) ;
#8190 = CARTESIAN_POINT('Ctrl Pts',(22.7891733238429,56.3978864499763,60.650151731163)) ;
#8191 = CARTESIAN_POINT('Ctrl Pts',(22.9568924415001,56.2965290899915,60.6386340110724)) ;
#8192 = CARTESIAN_POINT('Ctrl Pts',(22.61021664358,56.1295297083805,60.4709967147976)) ;
#8193 = CARTESIAN_POINT('Ctrl Pts',(22.6309062409902,56.1276240321524,60.6662120728825)) ;
#8194 = CARTESIAN_POINT('Ctrl Pts',(22.7983168419127,56.0262125668428,60.6511907273074)) ;
#8195 = CARTESIAN_POINT('Ctrl Pts',(22.2868305937246,55.5885108130465,60.5140535628389)) ;
#8196 = CARTESIAN_POINT('Ctrl Pts',(22.3156666086983,55.5866055506163,60.708230771592)) ;
#8197 = CARTESIAN_POINT('Ctrl Pts',(22.4823469794624,55.485272016298,60.6862170385931)) ;
#8198 = CARTESIAN_POINT('Ctrl Pts',(22.1258777321222,55.317901160658,60.5406410241412)) ;
#8199 = CARTESIAN_POINT('Ctrl Pts',(22.1587672526199,55.3159940909204,60.7341732409742)) ;
#8200 = CARTESIAN_POINT('Ctrl Pts',(22.3249457959597,55.214651875968,60.7086777753867)) ;
#8201 = CARTESIAN_POINT('Ctrl Pts',(21.8054571265389,54.7764805321528,60.6039693813565)) ;
#8202 = CARTESIAN_POINT('Ctrl Pts',(21.846418716765,54.7745728258528,60.7959584644911)) ;
#8203 = CARTESIAN_POINT('Ctrl Pts',(22.0113163449193,54.6731104541105,60.7635398914439)) ;
#8204 = CARTESIAN_POINT('Ctrl Pts',(21.6460058840883,54.5052712784107,60.6407300937437)) ;
#8205 = CARTESIAN_POINT('Ctrl Pts',(21.6909879829958,54.5033650627666,60.8318137773509)) ;
#8206 = CARTESIAN_POINT('Ctrl Pts',(21.8552392919195,54.402027181747,60.7959300556672)) ;
#8207 = CARTESIAN_POINT('Ctrl Pts',(21.3304302531076,53.9638812711429,60.723995284381)) ;
#8208 = CARTESIAN_POINT('Ctrl Pts',(21.3833666353325,53.961974913084,60.9130306639828)) ;
#8209 = CARTESIAN_POINT('Ctrl Pts',(21.5459580455397,53.8606102462171,60.8703104985783)) ;
#8210 = CARTESIAN_POINT('Ctrl Pts',(21.1739449590052,53.6935003224017,60.7705861098554)) ;
#8211 = CARTESIAN_POINT('Ctrl Pts',(21.2308267414169,53.6915946089307,60.9584728507535)) ;
#8212 = CARTESIAN_POINT('Ctrl Pts',(21.3924690809887,53.5901950776532,60.9123643251348)) ;
#8213 = CARTESIAN_POINT('Ctrl Pts',(20.8644295345407,53.1525885953574,60.8734112573306)) ;
#8214 = CARTESIAN_POINT('Ctrl Pts',(20.9291169100103,53.1506832357842,61.0587537283216)) ;
#8215 = CARTESIAN_POINT('Ctrl Pts',(21.0887268134599,53.0493503316648,61.0059167664191)) ;
#8216 = CARTESIAN_POINT('Ctrl Pts',(20.7114237625881,52.882199970333,60.9296260238961)) ;
#8217 = CARTESIAN_POINT('Ctrl Pts',(20.7799690600203,52.8802927777011,61.1135770768887)) ;
#8218 = CARTESIAN_POINT('Ctrl Pts',(20.9384318123433,52.7789455602561,61.05741757716)) ;
#8219 = CARTESIAN_POINT('Ctrl Pts',(20.4089174963609,52.3415574725868,61.0516641128343)) ;
#8220 = CARTESIAN_POINT('Ctrl Pts',(20.4850932611546,52.3396495857293,61.2325923658241)) ;
#8221 = CARTESIAN_POINT('Ctrl Pts',(20.6409989900421,52.2381712237815,61.1698828503062)) ;
#8222 = CARTESIAN_POINT('Ctrl Pts',(20.2595076558012,52.0708923183184,61.1174628765065)) ;
#8223 = CARTESIAN_POINT('Ctrl Pts',(20.3394548866061,52.0689860210861,61.2967525281003)) ;
#8224 = CARTESIAN_POINT('Ctrl Pts',(20.4940904813883,51.9676510264126,61.2307636933388)) ;
#8225 = CARTESIAN_POINT('Ctrl Pts',(19.9650527208262,51.5294526417529,61.2583331584609)) ;
#8226 = CARTESIAN_POINT('Ctrl Pts',(20.0524312593111,51.5275461441627,61.434121987783)) ;
#8227 = CARTESIAN_POINT('Ctrl Pts',(20.2041507845699,51.4261734610014,61.3617298195192)) ;
#8228 = CARTESIAN_POINT('Ctrl Pts',(19.8196993362125,51.2584285629725,61.3335698183793)) ;
#8229 = CARTESIAN_POINT('Ctrl Pts',(19.910747581436,51.2565228089847,61.5074867887763)) ;
#8230 = CARTESIAN_POINT('Ctrl Pts',(20.0609066761106,51.155134072336,61.431931527665)) ;
#8231 = CARTESIAN_POINT('Ctrl Pts',(19.5345636251539,50.716825622987,61.4927171177322)) ;
#8232 = CARTESIAN_POINT('Ctrl Pts',(19.6328117475426,50.7149201642453,61.6626689874544)) ;
#8233 = CARTESIAN_POINT('Ctrl Pts',(19.779704921468,50.6135869790364,61.5808800021285)) ;
#8234 = CARTESIAN_POINT('Ctrl Pts',(19.3946960746612,50.4462620313475,61.5766493945011)) ;
#8235 = CARTESIAN_POINT('Ctrl Pts',(19.4964757082143,50.4443547062501,61.7445107101472)) ;
#8236 = CARTESIAN_POINT('Ctrl Pts',(19.6416157612327,50.3430015532564,61.6596722673663)) ;
#8237 = CARTESIAN_POINT('Ctrl Pts',(19.120347271349,49.9056099883002,61.7532078208345)) ;
#8238 = CARTESIAN_POINT('Ctrl Pts',(19.2290575176146,49.9037019096545,61.9166704920289)) ;
#8239 = CARTESIAN_POINT('Ctrl Pts',(19.3704530768998,49.8022062837629,61.8258792263852)) ;
#8240 = CARTESIAN_POINT('Ctrl Pts',(18.9859992421676,49.6350408217894,61.8457599517748)) ;
#8241 = CARTESIAN_POINT('Ctrl Pts',(19.0981049563584,49.6331344367489,62.006907681661)) ;
#8242 = CARTESIAN_POINT('Ctrl Pts',(19.2376494534462,49.5318014383597,61.91312930125)) ;
#8243 = CARTESIAN_POINT('Ctrl Pts',(18.7234168960688,49.094225030673,62.0390565968025)) ;
#8244 = CARTESIAN_POINT('Ctrl Pts',(18.8421597145869,49.0923183861909,62.1953797257233)) ;
#8245 = CARTESIAN_POINT('Ctrl Pts',(18.9776400235437,48.9909365753488,62.0958671992294)) ;
#8246 = CARTESIAN_POINT('Ctrl Pts',(18.5950057536361,48.8238179925609,62.1399409713884)) ;
#8247 = CARTESIAN_POINT('Ctrl Pts',(18.7169956791222,48.8219121927132,62.2937435774521)) ;
#8248 = CARTESIAN_POINT('Ctrl Pts',(18.8503646589018,48.7205331729861,62.191416023735)) ;
#8249 = CARTESIAN_POINT('Ctrl Pts',(18.344791622651,48.2823982252904,62.3495579783263)) ;
#8250 = CARTESIAN_POINT('Ctrl Pts',(18.4731096558997,48.2804926625104,62.4981204671872)) ;
#8251 = CARTESIAN_POINT('Ctrl Pts',(18.6021004401867,48.1791582421601,62.3902864565594)) ;
#8252 = CARTESIAN_POINT('Ctrl Pts',(18.2228959649897,48.0114576298592,62.4583587669778)) ;
#8253 = CARTESIAN_POINT('Ctrl Pts',(18.3542987951968,48.0095520696155,62.6042054927202)) ;
#8254 = CARTESIAN_POINT('Ctrl Pts',(18.4809339819869,47.9080609643498,62.4937510691697)) ;
#8255 = CARTESIAN_POINT('Ctrl Pts',(17.9860167173073,47.4697670852059,62.6835784937478)) ;
#8256 = CARTESIAN_POINT('Ctrl Pts',(18.1234139395054,47.4678622559185,62.8237875200317)) ;
#8257 = CARTESIAN_POINT('Ctrl Pts',(18.2453689199781,47.3665093096488,62.7080713201897)) ;
#8258 = CARTESIAN_POINT('Ctrl Pts',(17.8713622037688,47.1991192501592,62.7996706789161)) ;
#8259 = CARTESIAN_POINT('Ctrl Pts',(18.0116612186128,47.1972127705363,62.9369749602238)) ;
#8260 = CARTESIAN_POINT('Ctrl Pts',(18.1311767720907,47.0958808569954,62.8187239599312)) ;
#8261 = CARTESIAN_POINT('Ctrl Pts',(17.6495728367388,46.6582159321309,63.0387734246909)) ;
#8262 = CARTESIAN_POINT('Ctrl Pts',(17.7954894043096,46.6563091331966,63.1700945757485)) ;
#8263 = CARTESIAN_POINT('Ctrl Pts',(17.909933212892,46.55491712217,63.0469754684038)) ;
#8264 = CARTESIAN_POINT('Ctrl Pts',(17.5423655416169,46.387893043845,63.1618809435582)) ;
#8265 = CARTESIAN_POINT('Ctrl Pts',(17.6909986176242,46.3859871917481,63.2901184799721)) ;
#8266 = CARTESIAN_POINT('Ctrl Pts',(17.8028497172398,46.2846172014538,63.1646224320618)) ;
#8267 = CARTESIAN_POINT('Ctrl Pts',(17.3360387404632,45.8470089936285,63.4143795876991)) ;
#8268 = CARTESIAN_POINT('Ctrl Pts',(17.4899015253219,45.8451033188971,63.5362916945355)) ;
#8269 = CARTESIAN_POINT('Ctrl Pts',(17.5964220062636,45.7437666877308,63.4062158185806)) ;
#8270 = CARTESIAN_POINT('Ctrl Pts',(17.2368458636899,45.5765948766505,63.5438417903575)) ;
#8271 = CARTESIAN_POINT('Ctrl Pts',(17.3932248689923,45.5746876691604,63.6625139851918)) ;
#8272 = CARTESIAN_POINT('Ctrl Pts',(17.4969830128249,45.4732994150383,63.530260528991)) ;
#8273 = CARTESIAN_POINT('Ctrl Pts',(17.1416766080821,45.3060601767044,63.6764864071842)) ;
#8274 = CARTESIAN_POINT('Ctrl Pts',(17.3004704348883,45.3041537286489,63.791833369093)) ;
#8275 = CARTESIAN_POINT('Ctrl Pts',(17.401402501053,45.2027271666488,63.6574852908108)) ;
#8276 = CARTESIAN_POINT('Ctrl Pts',(17.0490336577126,45.1993067880441,63.8123519660661)) ;
#8277 = CARTESIAN_POINT('Ctrl Pts',(17.2087077484269,45.2022941676425,63.9227233952561)) ;
#8278 = CARTESIAN_POINT('Ctrl Pts',(17.1177210656172,45.3026134137914,64.06180633622)) ;
#8279 = CARTESIAN_POINT('Ctrl Pts',(17.1455226949134,45.4820412744375,63.6716960182275)) ;
#8280 = CARTESIAN_POINT('Ctrl Pts',(17.3027834310888,45.4850270679756,63.7855615284192)) ;
#8281 = CARTESIAN_POINT('Ctrl Pts',(17.2087519082886,45.5853439255196,63.922655892153)) ;
#8282 = CARTESIAN_POINT('Ctrl Pts',(17.2464212678063,45.7643410734657,63.5345175445691)) ;
#8283 = CARTESIAN_POINT('Ctrl Pts',(17.401152681015,45.7673274764212,63.6517895025822)) ;
#8284 = CARTESIAN_POINT('Ctrl Pts',(17.3041243260271,45.8675609242035,63.7868355301742)) ;
#8285 = CARTESIAN_POINT('Ctrl Pts',(17.4565134656398,46.3280183067045,63.2675668339134)) ;
#8286 = CARTESIAN_POINT('Ctrl Pts',(17.6059910908437,46.331004915594,63.3914666923995)) ;
#8287 = CARTESIAN_POINT('Ctrl Pts',(17.5031785660295,46.4312549192417,63.5221510947456)) ;
#8288 = CARTESIAN_POINT('Ctrl Pts',(17.5658513791384,46.6093355962106,63.1376190987605)) ;
#8289 = CARTESIAN_POINT('Ctrl Pts',(17.7125968167087,46.6123217179431,63.2647451499116)) ;
#8290 = CARTESIAN_POINT('Ctrl Pts',(17.6069791740221,46.712617478714,63.3931394651388)) ;
#8291 = CARTESIAN_POINT('Ctrl Pts',(17.7924789756583,47.1717937445044,62.8854376933859)) ;
#8292 = CARTESIAN_POINT('Ctrl Pts',(17.9335562333469,47.1747789756612,63.0188226312906)) ;
#8293 = CARTESIAN_POINT('Ctrl Pts',(17.8224307838778,47.2750030883984,63.1425350068647)) ;
#8294 = CARTESIAN_POINT('Ctrl Pts',(17.9097228296802,47.4527838882153,62.7632359923575)) ;
#8295 = CARTESIAN_POINT('Ctrl Pts',(18.0478719290323,47.4557718391432,62.8996519815895)) ;
#8296 = CARTESIAN_POINT('Ctrl Pts',(17.9340906077666,47.5560106522166,63.0209148247748)) ;
#8297 = CARTESIAN_POINT('Ctrl Pts',(18.152046918103,48.0142871287591,62.5265870268212)) ;
#8298 = CARTESIAN_POINT('Ctrl Pts',(18.2841480165347,48.0172768213242,62.6688740735516)) ;
#8299 = CARTESIAN_POINT('Ctrl Pts',(18.165263429428,48.1176560532207,62.7850247741514)) ;
#8300 = CARTESIAN_POINT('Ctrl Pts',(18.2770385109489,48.2952668191048,62.4122452341964)) ;
#8301 = CARTESIAN_POINT('Ctrl Pts',(18.4060099207561,48.2982535238503,62.5573681352024)) ;
#8302 = CARTESIAN_POINT('Ctrl Pts',(18.2845680798083,48.3984774868501,62.6709705308533)) ;
#8303 = CARTESIAN_POINT('Ctrl Pts',(18.5341439279546,48.8569739450436,62.1919748252194)) ;
#8304 = CARTESIAN_POINT('Ctrl Pts',(18.6566967270201,48.8599612929924,62.3425595457133)) ;
#8305 = CARTESIAN_POINT('Ctrl Pts',(18.5304598910702,48.9602369846067,62.4507639370776)) ;
#8306 = CARTESIAN_POINT('Ctrl Pts',(18.6664510738312,49.1378578224521,62.0858933183196)) ;
#8307 = CARTESIAN_POINT('Ctrl Pts',(18.7856992455192,49.1408439740008,62.2391079338026)) ;
#8308 = CARTESIAN_POINT('Ctrl Pts',(18.6571347380458,49.2411084827289,62.3445461273707)) ;
#8309 = CARTESIAN_POINT('Ctrl Pts',(18.9376946500433,49.7002903800722,61.8825932573844)) ;
#8310 = CARTESIAN_POINT('Ctrl Pts',(19.050169723931,49.7032760750642,62.0408453671987)) ;
#8311 = CARTESIAN_POINT('Ctrl Pts',(18.9171280204917,49.803503874625,62.1406092424056)) ;
#8312 = CARTESIAN_POINT('Ctrl Pts',(19.0766896002932,49.981574104154,61.7853116649667)) ;
#8313 = CARTESIAN_POINT('Ctrl Pts',(19.1857006417587,49.9845603797215,61.9459752235339)) ;
#8314 = CARTESIAN_POINT('Ctrl Pts',(19.0505798995618,50.0849206295543,62.0427767583232)) ;
#8315 = CARTESIAN_POINT('Ctrl Pts',(19.3614455200386,50.5452598054505,61.599607012202)) ;
#8316 = CARTESIAN_POINT('Ctrl Pts',(19.4633446760807,50.5482445256743,61.7648678207392)) ;
#8317 = CARTESIAN_POINT('Ctrl Pts',(19.3240747731292,50.6484794513874,61.8557278637767)) ;
#8318 = CARTESIAN_POINT('Ctrl Pts',(19.5068971693961,50.8275371605432,61.5113786134476)) ;
#8319 = CARTESIAN_POINT('Ctrl Pts',(19.6051679348679,50.8305243023331,61.6788222555382)) ;
#8320 = CARTESIAN_POINT('Ctrl Pts',(19.4639424629956,50.9307473366981,61.7666251609937)) ;
#8321 = CARTESIAN_POINT('Ctrl Pts',(19.7297237719396,51.2516112326461,61.3860283416691)) ;
#8322 = CARTESIAN_POINT('Ctrl Pts',(19.8224379405654,51.2545984104599,61.5565744041528)) ;
#8323 = CARTESIAN_POINT('Ctrl Pts',(19.6784682413758,51.3548887142934,61.6396658154339)) ;
#8324 = CARTESIAN_POINT('Ctrl Pts',(19.8048505346244,51.3931523912137,61.3453731396617)) ;
#8325 = CARTESIAN_POINT('Ctrl Pts',(19.895690982332,51.3961391935501,61.5169252343388)) ;
#8326 = CARTESIAN_POINT('Ctrl Pts',(19.7508279665644,51.4964465474925,61.5984296343693)) ;
#8327 = CARTESIAN_POINT('Ctrl Pts',(19.9562473847284,51.6761627264631,61.2666350136366)) ;
#8328 = CARTESIAN_POINT('Ctrl Pts',(20.0433090702939,51.6791488679163,61.4401333749345)) ;
#8329 = CARTESIAN_POINT('Ctrl Pts',(19.896670741513,51.7794030062388,61.5184624170268)) ;
#8330 = CARTESIAN_POINT('Ctrl Pts',(20.0325166502847,51.8176028378205,61.2285471996139)) ;
#8331 = CARTESIAN_POINT('Ctrl Pts',(20.1176756133913,51.8205891355623,61.4029868205377)) ;
#8332 = CARTESIAN_POINT('Ctrl Pts',(19.9701828553007,51.9208298261689,61.4797112591545)) ;
#8333 = CARTESIAN_POINT('Ctrl Pts',(20.2630296190609,52.2417288193162,61.1181108441885)) ;
#8334 = CARTESIAN_POINT('Ctrl Pts',(20.3424395047616,52.2447151365725,61.2952797212327)) ;
#8335 = CARTESIAN_POINT('Ctrl Pts',(20.1924847498882,52.3449566194198,61.3671412503005)) ;
#8336 = CARTESIAN_POINT('Ctrl Pts',(20.4190843256942,52.5241300049794,61.0495422547059)) ;
#8337 = CARTESIAN_POINT('Ctrl Pts',(20.4946049613182,52.5271161388784,61.2284060668257)) ;
#8338 = CARTESIAN_POINT('Ctrl Pts',(20.3431512476579,52.6274277787848,61.2969560666953)) ;
#8339 = CARTESIAN_POINT('Ctrl Pts',(20.7352774289549,53.089174481225,60.9228046908309)) ;
#8340 = CARTESIAN_POINT('Ctrl Pts',(20.8029106375314,53.0921595377318,61.1047944240417)) ;
#8341 = CARTESIAN_POINT('Ctrl Pts',(20.6485625806559,53.1923844744817,61.1666835299605)) ;
#8342 = CARTESIAN_POINT('Ctrl Pts',(20.8952932693716,53.3716654702891,60.8646724123074)) ;
#8343 = CARTESIAN_POINT('Ctrl Pts',(20.958939113703,53.3746531996274,61.0480949606972)) ;
#8344 = CARTESIAN_POINT('Ctrl Pts',(20.8032801065143,53.4748857690477,61.1065967793017)) ;
#8345 = CARTESIAN_POINT('Ctrl Pts',(21.2191660762763,53.9365848433116,60.7588866402754)) ;
#8346 = CARTESIAN_POINT('Ctrl Pts',(21.2747437665872,53.9395741566696,60.9449172512699)) ;
#8347 = CARTESIAN_POINT('Ctrl Pts',(21.1167457369649,54.0399343658719,60.9965396864954)) ;
#8348 = CARTESIAN_POINT('Ctrl Pts',(21.3829591038786,54.2194050937958,60.7112697291679)) ;
#8349 = CARTESIAN_POINT('Ctrl Pts',(21.4344485275877,54.2223916876299,60.8984685858512)) ;
#8350 = CARTESIAN_POINT('Ctrl Pts',(21.2752873587406,54.322617764982,60.9466468381776)) ;
#8351 = CARTESIAN_POINT('Ctrl Pts',(21.7134230274786,54.7853172886335,60.6268523737491)) ;
#8352 = CARTESIAN_POINT('Ctrl Pts',(21.7566785748286,54.7883043794258,60.8161247816509)) ;
#8353 = CARTESIAN_POINT('Ctrl Pts',(21.5955845359118,54.8885704142163,60.8572908231305)) ;
#8354 = CARTESIAN_POINT('Ctrl Pts',(21.8802808706122,55.0683374452623,60.5900200604226)) ;
#8355 = CARTESIAN_POINT('Ctrl Pts',(21.9193783050032,55.0713235719889,60.7801950956779)) ;
#8356 = CARTESIAN_POINT('Ctrl Pts',(21.7574250730561,55.1715968138679,60.8178208957825)) ;
#8357 = CARTESIAN_POINT('Ctrl Pts',(22.2153336537663,55.6338317486076,60.5275072380942)) ;
#8358 = CARTESIAN_POINT('Ctrl Pts',(22.2460816167474,55.6368172834239,60.7192077956619)) ;
#8359 = CARTESIAN_POINT('Ctrl Pts',(22.0826126303576,55.7370429277275,60.7497260223226)) ;
#8360 = CARTESIAN_POINT('Ctrl Pts',(22.3836539671604,55.9162154787364,60.5017754298194)) ;
#8361 = CARTESIAN_POINT('Ctrl Pts',(22.4102134039785,55.9192018042841,60.6941060183188)) ;
#8362 = CARTESIAN_POINT('Ctrl Pts',(22.2461996794021,56.0195762764982,60.7210326751055)) ;
#8363 = CARTESIAN_POINT('Ctrl Pts',(22.7220464748074,56.4812254904543,60.461349008304)) ;
#8364 = CARTESIAN_POINT('Ctrl Pts',(22.740172194055,56.4842101348188,60.6546523260149)) ;
#8365 = CARTESIAN_POINT('Ctrl Pts',(22.5750628838645,56.5844490941092,60.6743976159306)) ;
#8366 = CARTESIAN_POINT('Ctrl Pts',(22.8916830507608,56.7637439358806,60.4467024834945)) ;
#8367 = CARTESIAN_POINT('Ctrl Pts',(22.9055849340659,56.7667309512735,60.6403547970455)) ;
#8368 = CARTESIAN_POINT('Ctrl Pts',(22.7400743833527,56.8669533046418,60.6564901223893)) ;
#8369 = CARTESIAN_POINT('Ctrl Pts',(23.2318362481627,57.3288079962322,60.428527054267)) ;
#8370 = CARTESIAN_POINT('Ctrl Pts',(23.2372699125271,57.3317959922072,60.6226042851211)) ;
#8371 = CARTESIAN_POINT('Ctrl Pts',(23.0712569554089,57.4320972449965,60.6314923959532)) ;
#8372 = CARTESIAN_POINT('Ctrl Pts',(23.4024476603049,57.611503670388,60.4250093486565)) ;
#8373 = CARTESIAN_POINT('Ctrl Pts',(23.4036306456897,57.6144899220688,60.6191573059636)) ;
#8374 = CARTESIAN_POINT('Ctrl Pts',(23.2374315995444,57.7147356136583,60.624412729286)) ;
#8375 = CARTESIAN_POINT('Ctrl Pts',(23.7435444880125,58.1775332619085,60.4291798819412)) ;
#8376 = CARTESIAN_POINT('Ctrl Pts',(23.7362349072975,58.1805194049396,60.623193506534)) ;
#8377 = CARTESIAN_POINT('Ctrl Pts',(23.5699601204502,58.2807563670397,60.6211751413546)) ;
#8378 = CARTESIAN_POINT('Ctrl Pts',(23.9141929541263,58.4605262973812,60.4368761160161)) ;
#8379 = CARTESIAN_POINT('Ctrl Pts',(23.9026365192723,58.4635110441036,60.6306861729615)) ;
#8380 = CARTESIAN_POINT('Ctrl Pts',(23.7365085092164,58.5638587343536,60.6250289006596)) ;
#8381 = CARTESIAN_POINT('Ctrl Pts',(24.0840192284084,58.7433256931628,60.4501282929911)) ;
#8382 = CARTESIAN_POINT('Ctrl Pts',(24.0682327693193,58.7463119239391,60.6435880950894)) ;
#8383 = CARTESIAN_POINT('Ctrl Pts',(23.9022262800894,58.846513767945,60.634300421317)) ;
#8384 = CARTESIAN_POINT('Origin',(-4.80851752474837,45.3830586252741,88.8353684199565)) ;
#8385 = CARTESIAN_POINT('',(17.1688786268051,45.3830610445957,72.8060570186675)) ;
#8386 = CARTESIAN_POINT('',(0.569856645481987,45.3830586252741,84.8659474548835)) ;
#8387 = CARTESIAN_POINT('',(17.1688762698447,45.3830586252741,72.8060537745881)) ;
#8388 = CARTESIAN_POINT('Ctrl Pts',(17.1688794847748,45.3830586252741,72.8060581995622)) ;
#8389 = CARTESIAN_POINT('Ctrl Pts',(17.1800655091625,45.3830586252741,72.7979310784706)) ;
#8390 = CARTESIAN_POINT('Ctrl Pts',(17.1901949893514,45.3830586252741,72.7885022675957)) ;
#8391 = CARTESIAN_POINT('Ctrl Pts',(17.2087915183656,45.3830586252741,72.7665630539906)) ;
#8392 = CARTESIAN_POINT('Ctrl Pts',(17.2169373449558,45.3830586252741,72.7540141333136)) ;
#8393 = CARTESIAN_POINT('Ctrl Pts',(17.2355140967823,45.3830586252741,72.7162404357135)) ;
#8394 = CARTESIAN_POINT('Ctrl Pts',(17.2421115176057,45.3830586252741,72.6895919213799)) ;
#8395 = CARTESIAN_POINT('Ctrl Pts',(17.2455991389693,45.3830586252741,72.6330329519167)) ;
#8396 = CARTESIAN_POINT('Ctrl Pts',(17.2416418239109,45.3830586252736,72.6034108053733)) ;
#8397 = CARTESIAN_POINT('Ctrl Pts',(17.2249824939971,45.3830586252736,72.5497711522179)) ;
#8398 = CARTESIAN_POINT('Ctrl Pts',(17.2131755915674,45.3830586252741,72.5255254786368)) ;
#8399 = CARTESIAN_POINT('Ctrl Pts',(17.1981507140927,45.3830586252741,72.5034867616281)) ;
#8400 = CARTESIAN_POINT('',(17.2299597049927,45.3830674541111,72.8852989434337)) ;
#8401 = CARTESIAN_POINT('Ctrl Pts',(17.5258214295105,45.3830586252741,72.9484557918475)) ;
#8402 = CARTESIAN_POINT('Ctrl Pts',(17.5095041570387,45.3830586252741,72.9279068266439)) ;
#8403 = CARTESIAN_POINT('Ctrl Pts',(17.4902242692681,45.3830586252745,72.9096981137126)) ;
#8404 = CARTESIAN_POINT('Ctrl Pts',(17.4444073336212,45.3830586252745,72.8778489307896)) ;
#8405 = CARTESIAN_POINT('Ctrl Pts',(17.4172953260424,45.3830586252741,72.8651171123935)) ;
#8406 = CARTESIAN_POINT('Ctrl Pts',(17.3621978432612,45.3830586252741,72.8513607012809)) ;
#8407 = CARTESIAN_POINT('Ctrl Pts',(17.3347399628247,45.3830586252741,72.849611691816)) ;
#8408 = CARTESIAN_POINT('Ctrl Pts',(17.2932911066477,45.3830586252741,72.8559099542529)) ;
#8409 = CARTESIAN_POINT('Ctrl Pts',(17.2790818332707,45.3830586252741,72.8598039396343)) ;
#8410 = CARTESIAN_POINT('Ctrl Pts',(17.2529022556706,45.3830586252741,72.8706466438317)) ;
#8411 = CARTESIAN_POINT('Ctrl Pts',(17.2409892021835,45.3830586252741,72.8772920314038)) ;
#8412 = CARTESIAN_POINT('Ctrl Pts',(17.2299628898897,45.3830586252741,72.8853032108675)) ;
#8413 = CARTESIAN_POINT('',(1.58245214009829,45.3830586252741,84.2538605621281)) ;
#8414 = CARTESIAN_POINT('',(1.58245214009829,45.3830586252741,84.2538605621281)) ;
#8415 = CARTESIAN_POINT('Origin',(-2.53204462594907,45.3830586252741,78.5907416015035)) ;
#8416 = CARTESIAN_POINT('Ctrl Pts',(17.4100634185147,45.3830502402116,72.6308270694242)) ;
#8417 = CARTESIAN_POINT('Ctrl Pts',(17.2062496612647,45.9804808943695,72.3503018815983)) ;
#8418 = CARTESIAN_POINT('Ctrl Pts',(17.0291891298972,46.5779115664506,72.0521676888577)) ;
#8419 = CARTESIAN_POINT('Ctrl Pts',(16.8521298437262,47.1753380370388,71.7540355927766)) ;
#8420 = CARTESIAN_POINT('Ctrl Pts',(16.703334020664,47.772764507627,71.4408383057955)) ;
#8421 = CARTESIAN_POINT('Ctrl Pts',(16.5545381976019,48.3701909782152,71.1276410188143)) ;
#8422 = CARTESIAN_POINT('Ctrl Pts',(16.435275311147,48.9676174488035,70.8020506297554)) ;
#8423 = CARTESIAN_POINT('Ctrl Pts',(16.3160124246922,49.5650439193917,70.4764602406964)) ;
#8424 = CARTESIAN_POINT('Ctrl Pts',(16.2272999837411,50.16247038998,70.1412545719592)) ;
#8425 = CARTESIAN_POINT('Ctrl Pts',(16.1385875427899,50.7598968605682,69.8060489032219)) ;
#8426 = CARTESIAN_POINT('Ctrl Pts',(16.0811824106094,51.3573233311564,69.4640878113819)) ;
#8427 = CARTESIAN_POINT('Ctrl Pts',(16.023777278429,51.9547498017447,69.1221267195418)) ;
#8428 = CARTESIAN_POINT('Ctrl Pts',(15.9981692153665,52.5521762723329,68.7763276960625)) ;
#8429 = CARTESIAN_POINT('Ctrl Pts',(15.9725611523041,53.1496027429211,68.4305286725831)) ;
#8430 = CARTESIAN_POINT('Ctrl Pts',(15.9789686373246,53.7470292135094,68.0838419528074)) ;
#8431 = CARTESIAN_POINT('Ctrl Pts',(15.985376122345,54.3444556840976,67.7371552330318)) ;
#8432 = CARTESIAN_POINT('Ctrl Pts',(16.0237444890454,54.9418821546858,67.3925386258147)) ;
#8433 = CARTESIAN_POINT('Ctrl Pts',(16.0621128557458,55.5393086252741,67.0479220185975)) ;
#8434 = CARTESIAN_POINT('Ctrl Pts',(16.1321147587497,56.1367350958623,66.7083156713233)) ;
#8435 = CARTESIAN_POINT('Ctrl Pts',(16.2021166617536,56.7341615664506,66.3687093240491)) ;
#8436 = CARTESIAN_POINT('Ctrl Pts',(16.3031548695066,57.3315880370388,66.037010638331)) ;
#8437 = CARTESIAN_POINT('Ctrl Pts',(16.3920498868663,57.8572133193466,65.7451768748386)) ;
#8438 = CARTESIAN_POINT('Ctrl Pts',(16.5043534680133,58.3830758086166,65.4615271343363)) ;
#8439 = CARTESIAN_POINT('Ctrl Pts',(-4.83789343805113,45.3830502402116,88.7949359439767)) ;
#8440 = CARTESIAN_POINT('Ctrl Pts',(-5.78902430521799,45.9804808943695,87.4858184007887)) ;
#8441 = CARTESIAN_POINT('Ctrl Pts',(-6.6153067849329,46.5779115664506,86.0945255013329)) ;
#8442 = CARTESIAN_POINT('Ctrl Pts',(-7.44158345373106,47.1753380370388,84.7032423862879)) ;
#8443 = CARTESIAN_POINT('Ctrl Pts',(-8.13596396135441,47.772764507627,83.2416550470425)) ;
#8444 = CARTESIAN_POINT('Ctrl Pts',(-8.83034446897775,48.3701909782152,81.7800677077971)) ;
#8445 = CARTESIAN_POINT('Ctrl Pts',(-9.38690460576691,48.9676174488035,80.2606458921887)) ;
#8446 = CARTESIAN_POINT('Ctrl Pts',(-9.94346474255606,49.5650439193917,78.7412240765802)) ;
#8447 = CARTESIAN_POINT('Ctrl Pts',(-10.3574561336615,50.16247038998,77.1769309558065)) ;
#8448 = CARTESIAN_POINT('Ctrl Pts',(-10.771447524767,50.7598968605682,75.6126378350327)) ;
#8449 = CARTESIAN_POINT('Ctrl Pts',(-11.0393381416091,51.3573233311564,74.0168194064458)) ;
#8450 = CARTESIAN_POINT('Ctrl Pts',(-11.3072287584512,51.9547498017447,72.4210009778589)) ;
#8451 = CARTESIAN_POINT('Ctrl Pts',(-11.4267330527426,52.5521762723329,70.8072722016218)) ;
#8452 = CARTESIAN_POINT('Ctrl Pts',(-11.546237347034,53.1496027429211,69.1935434253848)) ;
#8453 = CARTESIAN_POINT('Ctrl Pts',(-11.5163357502719,53.7470292135094,67.5756720664317)) ;
#8454 = CARTESIAN_POINT('Ctrl Pts',(-11.4864341535098,54.3444556840976,65.9578007074786)) ;
#8455 = CARTESIAN_POINT('Ctrl Pts',(-11.3073817755747,54.9418821546858,64.3495898737987)) ;
#8456 = CARTESIAN_POINT('Ctrl Pts',(-11.1283293976396,55.5393086252741,62.7413790401188)) ;
#8457 = CARTESIAN_POINT('Ctrl Pts',(-10.8016538502879,56.1367350958623,61.1565494195059)) ;
#8458 = CARTESIAN_POINT('Ctrl Pts',(-10.4749783029363,56.7341615664506,59.5717197988929)) ;
#8459 = CARTESIAN_POINT('Ctrl Pts',(-10.0034666667556,57.3315880370388,58.0237925988748)) ;
#8460 = CARTESIAN_POINT('Ctrl Pts',(-9.5886232524106,57.8572133193466,56.6619017025771)) ;
#8461 = CARTESIAN_POINT('Ctrl Pts',(-9.06453987372463,58.3830758086166,55.3382029135661)) ;
#8462 = CARTESIAN_POINT('',(-1.74213662306825,58.3353824278239,58.3447753707129)) ;
#8463 = CARTESIAN_POINT('',(16.1909549772416,58.2172712656977,65.4449915594351)) ;
#8464 = CARTESIAN_POINT('Ctrl Pts',(-1.74213662306824,58.3353824278239,58.3447753707129)) ;
#8465 = CARTESIAN_POINT('Ctrl Pts',(0.655926738612619,58.3308357090662,59.2942358214405)) ;
#8466 = CARTESIAN_POINT('Ctrl Pts',(3.34356255401777,58.3244410141138,60.3583461170491)) ;
#8467 = CARTESIAN_POINT('Ctrl Pts',(7.96103805230599,58.3066351840461,62.1865339947686)) ;
#8468 = CARTESIAN_POINT('Ctrl Pts',(13.032674621552,58.2895264446023,64.1945369607899)) ;
#8469 = CARTESIAN_POINT('Ctrl Pts',(16.1909559533793,58.2172696107886,65.4449889983622)) ;
#8470 = CARTESIAN_POINT('Ctrl Pts',(16.1909549772416,58.2172712656977,65.4449915594351)) ;
#8471 = CARTESIAN_POINT('Ctrl Pts',(16.1334478652878,57.9495340002375,65.5958675064122)) ;
#8472 = CARTESIAN_POINT('Ctrl Pts',(16.080655138304,57.6819084045915,65.7484708734625)) ;
#8473 = CARTESIAN_POINT('Ctrl Pts',(16.0326859680853,57.4145313636589,65.9024028922281)) ;
#8474 = CARTESIAN_POINT('Ctrl Pts',(15.9881564338053,57.1663266301679,66.0452971944471)) ;
#8475 = CARTESIAN_POINT('Ctrl Pts',(15.947768065655,56.9182638872712,66.189377214873)) ;
#8476 = CARTESIAN_POINT('Ctrl Pts',(15.9115671974444,56.6702295478714,66.3344521043164)) ;
#8477 = CARTESIAN_POINT('Ctrl Pts',(15.9087709003504,56.6510704023379,66.3456582579757)) ;
#8478 = CARTESIAN_POINT('Ctrl Pts',(15.9059993799389,56.6319118940954,66.3568711437602)) ;
#8479 = CARTESIAN_POINT('Ctrl Pts',(15.9032526664099,56.6127538456679,66.3680906454984)) ;
#8480 = CARTESIAN_POINT('Ctrl Pts',(15.8672287819349,56.3614909032359,66.5152374193485)) ;
#8481 = CARTESIAN_POINT('Ctrl Pts',(15.8354773115596,56.1103350670462,66.6635060977565)) ;
#8482 = CARTESIAN_POINT('Ctrl Pts',(15.8080789997499,55.8590202585561,66.8125541649163)) ;
#8483 = CARTESIAN_POINT('Ctrl Pts',(15.8063435636936,55.8431017310511,66.8219950162967)) ;
#8484 = CARTESIAN_POINT('Ctrl Pts',(15.8046256056966,55.8271830724927,66.8314387157162)) ;
#8485 = CARTESIAN_POINT('Ctrl Pts',(15.8029251298318,55.8112643008986,66.8408852528386)) ;
#8486 = CARTESIAN_POINT('Ctrl Pts',(15.7757327417881,55.5567064895585,66.9919452639956)) ;
#8487 = CARTESIAN_POINT('Ctrl Pts',(15.7529984536135,55.3019957844106,67.1438046094493)) ;
#8488 = CARTESIAN_POINT('Ctrl Pts',(15.7347441072865,55.0471908391173,67.296431137788)) ;
#8489 = CARTESIAN_POINT('Ctrl Pts',(15.7338348512874,55.034498906963,67.3040335237636)) ;
#8490 = CARTESIAN_POINT('Ctrl Pts',(15.7329367612736,55.0218058655745,67.3116377919328)) ;
#8491 = CARTESIAN_POINT('Ctrl Pts',(15.7320498443767,55.0091118266697,67.3192438421358)) ;
#8492 = CARTESIAN_POINT('Ctrl Pts',(15.7140153711204,54.7509925981973,67.4739044529036)) ;
#8493 = CARTESIAN_POINT('Ctrl Pts',(15.7006099199141,54.4926055130988,67.6292151883789)) ;
#8494 = CARTESIAN_POINT('Ctrl Pts',(15.6918744372802,54.2345762733044,67.7845220130878)) ;
#8495 = CARTESIAN_POINT('Ctrl Pts',(15.6915555684979,54.2251575070004,67.7901911329461)) ;
#8496 = CARTESIAN_POINT('Ctrl Pts',(15.6912428906292,54.2157389752755,67.7958606956662)) ;
#8497 = CARTESIAN_POINT('Ctrl Pts',(15.6909364038727,54.2063206495465,67.8015306898383)) ;
#8498 = CARTESIAN_POINT('Ctrl Pts',(15.6824344247839,53.9450551732693,67.9588170027652)) ;
#8499 = CARTESIAN_POINT('Ctrl Pts',(15.6787014922471,53.6840579939704,68.1163692599084)) ;
#8500 = CARTESIAN_POINT('Ctrl Pts',(15.6797376472066,53.4230444575824,68.2737467183678)) ;
#8501 = CARTESIAN_POINT('Ctrl Pts',(15.6797621169394,53.4168803877747,68.2774633288299)) ;
#8502 = CARTESIAN_POINT('Ctrl Pts',(15.6797892402505,53.4107163826999,68.2811798266539)) ;
#8503 = CARTESIAN_POINT('Ctrl Pts',(15.6798190170839,53.4045524432163,68.2848962113249)) ;
#8504 = CARTESIAN_POINT('Ctrl Pts',(15.6810956661459,53.1402803009609,68.4442321264586)) ;
#8505 = CARTESIAN_POINT('Ctrl Pts',(15.6872500775662,52.8760533725399,68.6034054826552)) ;
#8506 = CARTESIAN_POINT('Ctrl Pts',(15.6982860026285,52.6118787196959,68.7624120508549)) ;
#8507 = CARTESIAN_POINT('Ctrl Pts',(15.7095641185038,52.3419065760594,68.9249081253533)) ;
#8508 = CARTESIAN_POINT('Ctrl Pts',(15.7259450053447,52.0715787920596,69.0871364559427)) ;
#8509 = CARTESIAN_POINT('Ctrl Pts',(15.7473979457536,51.8011908422987,69.248727102498)) ;
#8510 = CARTESIAN_POINT('Ctrl Pts',(15.7474248784871,51.8008513882914,69.2489299687594)) ;
#8511 = CARTESIAN_POINT('Ctrl Pts',(15.7474518192137,51.8005119341974,69.249132834011)) ;
#8512 = CARTESIAN_POINT('Ctrl Pts',(15.7474787679334,51.8001724800174,69.2493356982519)) ;
#8513 = CARTESIAN_POINT('Ctrl Pts',(15.768687011999,51.5330270582814,69.4089868570238)) ;
#8514 = CARTESIAN_POINT('Ctrl Pts',(15.7949064956035,51.265585354454,69.5683471237062)) ;
#8515 = CARTESIAN_POINT('Ctrl Pts',(15.825976232437,50.9984015502859,69.7264176065219)) ;
#8516 = CARTESIAN_POINT('Ctrl Pts',(15.8263938754657,50.9948100344075,69.7285424084002)) ;
#8517 = CARTESIAN_POINT('Ctrl Pts',(15.8268123967231,50.9912185474961,69.7306669877117)) ;
#8518 = CARTESIAN_POINT('Ctrl Pts',(15.8272317958496,50.9876270907846,69.7327913420942)) ;
#8519 = CARTESIAN_POINT('Ctrl Pts',(15.8580524204697,50.7236996475837,69.8889049933665)) ;
#8520 = CARTESIAN_POINT('Ctrl Pts',(15.8936084612277,50.4599498020535,70.0438872783466)) ;
#8521 = CARTESIAN_POINT('Ctrl Pts',(15.9338929720513,50.1963788513667,70.1977390376298)) ;
#8522 = CARTESIAN_POINT('Ctrl Pts',(15.9349345190615,50.1895642834339,70.2017168404282)) ;
#8523 = CARTESIAN_POINT('Ctrl Pts',(15.9359792010563,50.1827500045963,70.205693788537)) ;
#8524 = CARTESIAN_POINT('Ctrl Pts',(15.9370270183765,50.175936008737,70.2096698856566)) ;
#8525 = CARTESIAN_POINT('Ctrl Pts',(15.9770577136676,49.915614875762,70.3615722537204)) ;
#8526 = CARTESIAN_POINT('Ctrl Pts',(16.021633457865,49.6552611188172,70.51209499173)) ;
#8527 = CARTESIAN_POINT('Ctrl Pts',(16.0707233750742,49.3948957256021,70.6611910631829)) ;
#8528 = CARTESIAN_POINT('Ctrl Pts',(16.0726253546305,49.3848079176934,70.6669677622679)) ;
#8529 = CARTESIAN_POINT('Ctrl Pts',(16.0745340756922,49.3747203101762,70.6727421930359)) ;
#8530 = CARTESIAN_POINT('Ctrl Pts',(16.0764495328902,49.3646329259558,70.6785143401714)) ;
#8531 = CARTESIAN_POINT('Ctrl Pts',(16.1252659004566,49.1075509841677,70.8256203452038)) ;
#8532 = CARTESIAN_POINT('Ctrl Pts',(16.1785286510604,48.8504690628025,70.9714340403597)) ;
#8533 = CARTESIAN_POINT('Ctrl Pts',(16.2360875883058,48.5931578990175,71.1155086094327)) ;
#8534 = CARTESIAN_POINT('Ctrl Pts',(16.2390736559674,48.5798089981879,71.1229829727923)) ;
#8535 = CARTESIAN_POINT('Ctrl Pts',(16.2420713782267,48.5664590689811,71.1304528859902)) ;
#8536 = CARTESIAN_POINT('Ctrl Pts',(16.2450807296188,48.553108105864,71.1379182711826)) ;
#8537 = CARTESIAN_POINT('Ctrl Pts',(16.302355237528,48.2990102146508,71.2800008024469)) ;
#8538 = CARTESIAN_POINT('Ctrl Pts',(16.3638763057718,48.0446012919296,71.4205384228564)) ;
#8539 = CARTESIAN_POINT('Ctrl Pts',(16.4295089824108,47.7903648312085,71.5591745911328)) ;
#8540 = CARTESIAN_POINT('Ctrl Pts',(16.4337903177685,47.7737805380753,71.5682180731221)) ;
#8541 = CARTESIAN_POINT('Ctrl Pts',(16.4380893087519,47.7571963611372,71.5772538003855)) ;
#8542 = CARTESIAN_POINT('Ctrl Pts',(16.4424059394334,47.7406123516807,71.5862817190454)) ;
#8543 = CARTESIAN_POINT('Ctrl Pts',(16.5077400019093,47.4896062337423,71.7229231519758)) ;
#8544 = CARTESIAN_POINT('Ctrl Pts',(16.5769345851249,47.2387261489801,71.8574206887935)) ;
#8545 = CARTESIAN_POINT('Ctrl Pts',(16.649994480359,46.9878897404754,71.9898280933001)) ;
#8546 = CARTESIAN_POINT('Ctrl Pts',(16.6557445125371,46.968148165214,72.000248951886)) ;
#8547 = CARTESIAN_POINT('Ctrl Pts',(16.6615183268011,46.9484074501544,72.0106565466277)) ;
#8548 = CARTESIAN_POINT('Ctrl Pts',(16.6673159147512,46.9286675886394,72.0210508865765)) ;
#8549 = CARTESIAN_POINT('Ctrl Pts',(16.7400494655528,46.6810214584449,72.1514529191488)) ;
#8550 = CARTESIAN_POINT('Ctrl Pts',(16.816583194872,46.4334531760668,72.2798518018417)) ;
#8551 = CARTESIAN_POINT('Ctrl Pts',(16.8967060985225,46.1857600468479,72.4058931251787)) ;
#8552 = CARTESIAN_POINT('Ctrl Pts',(16.9040710432613,46.1629919477681,72.4174789182401)) ;
#8553 = CARTESIAN_POINT('Ctrl Pts',(16.9114664718038,46.1402223084085,72.4290450372909)) ;
#8554 = CARTESIAN_POINT('Ctrl Pts',(16.918892209119,46.1174510138863,72.4405911830445)) ;
#8555 = CARTESIAN_POINT('Ctrl Pts',(16.9986900450414,45.8727480373458,72.5646674067618)) ;
#8556 = CARTESIAN_POINT('Ctrl Pts',(17.0820250603088,45.6279743432131,72.6865119727705)) ;
#8557 = CARTESIAN_POINT('Ctrl Pts',(17.1688786268051,45.3830610445957,72.8060570186675)) ;
#8558 = CARTESIAN_POINT('',(-9.01576415853505,48.5844537758935,81.2291845178394)) ;
#8559 = CARTESIAN_POINT('Ctrl Pts',(0.569856645481997,45.3830586252741,84.8659474548835)) ;
#8560 = CARTESIAN_POINT('Ctrl Pts',(0.101768125792855,45.4231929016305,85.0973286092697)) ;
#8561 = CARTESIAN_POINT('Ctrl Pts',(-0.388741206423391,45.4870033446879,85.2745890054788)) ;
#8562 = CARTESIAN_POINT('Ctrl Pts',(-1.40461265481983,45.6539797372436,85.5194765725832)) ;
#8563 = CARTESIAN_POINT('Ctrl Pts',(-1.92697987875259,45.7573388893142,85.5840021976)) ;
#8564 = CARTESIAN_POINT('Ctrl Pts',(-3.36578195558735,46.0833507061679,85.6012198119695)) ;
#8565 = CARTESIAN_POINT('Ctrl Pts',(-4.26787911740062,46.3336877227692,85.4315724216581)) ;
#8566 = CARTESIAN_POINT('Ctrl Pts',(-6.01413017476312,46.9107591797134,84.7414207150381)) ;
#8567 = CARTESIAN_POINT('Ctrl Pts',(-6.83158725253899,47.2383195349503,84.1982764868229)) ;
#8568 = CARTESIAN_POINT('Ctrl Pts',(-8.15849876575339,47.9083523080808,82.8562179605577)) ;
#8569 = CARTESIAN_POINT('Ctrl Pts',(-8.66956683354584,48.2450338483642,82.0799311245838)) ;
#8570 = CARTESIAN_POINT('Ctrl Pts',(-9.01576415853505,48.5844537758935,81.2291845178394)) ;
#8571 = CARTESIAN_POINT('',(-9.03437826004907,48.6029307720944,81.1827788925151)) ;
#8572 = CARTESIAN_POINT('Origin',(-42.1505219076146,48.3660423604261,94.3834385474725)) ;
#8573 = CARTESIAN_POINT('',(-11.2680762515848,55.0677871747466,64.0109179234559)) ;
#8574 = CARTESIAN_POINT('Ctrl Pts',(-9.03437826004907,48.6029307720944,81.1827788925151)) ;
#8575 = CARTESIAN_POINT('Ctrl Pts',(-9.21711120032186,48.785356686239,80.7241857458836)) ;
#8576 = CARTESIAN_POINT('Ctrl Pts',(-9.38690460576691,48.9676174488035,80.2606458921887)) ;
#8577 = CARTESIAN_POINT('Ctrl Pts',(-9.94346474255606,49.5650439193917,78.7412240765802)) ;
#8578 = CARTESIAN_POINT('Ctrl Pts',(-10.3574561336615,50.16247038998,77.1769309558065)) ;
#8579 = CARTESIAN_POINT('Ctrl Pts',(-10.771447524767,50.7598968605682,75.6126378350327)) ;
#8580 = CARTESIAN_POINT('Ctrl Pts',(-11.0393381416091,51.3573233311564,74.0168194064458)) ;
#8581 = CARTESIAN_POINT('Ctrl Pts',(-11.3072287584512,51.9547498017447,72.4210009778589)) ;
#8582 = CARTESIAN_POINT('Ctrl Pts',(-11.4267330527426,52.5521762723329,70.8072722016218)) ;
#8583 = CARTESIAN_POINT('Ctrl Pts',(-11.546237347034,53.1496027429211,69.1935434253848)) ;
#8584 = CARTESIAN_POINT('Ctrl Pts',(-11.5163357502719,53.7470292135094,67.5756720664317)) ;
#8585 = CARTESIAN_POINT('Ctrl Pts',(-11.4864341535098,54.3444556840976,65.9578007074786)) ;
#8586 = CARTESIAN_POINT('Ctrl Pts',(-11.3073817755747,54.9418821546858,64.3495898737987)) ;
#8587 = CARTESIAN_POINT('Ctrl Pts',(-11.2885183223426,55.0048219850164,64.1801623007153)) ;
#8588 = CARTESIAN_POINT('Ctrl Pts',(-11.2680762515848,55.0677871747466,64.0109179234559)) ;
#8589 = CARTESIAN_POINT('',(-11.2619535028072,55.0862551252693,63.9612945541202)) ;
#8590 = CARTESIAN_POINT('Origin',(-46.060912756941,55.539936013522,59.793693489166)) ;
#8591 = CARTESIAN_POINT('Ctrl Pts',(-11.2619535028072,55.0862551252693,63.9612945541202)) ;
#8592 = CARTESIAN_POINT('Ctrl Pts',(-11.1929984329768,55.2861476427457,63.4245274809913)) ;
#8593 = CARTESIAN_POINT('Ctrl Pts',(-11.0619746721449,55.4856144064207,62.8971457747828)) ;
#8594 = CARTESIAN_POINT('Ctrl Pts',(-10.6668298706646,55.8948727823204,61.8461329491164)) ;
#8595 = CARTESIAN_POINT('Ctrl Pts',(-10.3950419897871,56.1030297966037,61.3286333190244)) ;
#8596 = CARTESIAN_POINT('Ctrl Pts',(-9.51301503825525,56.6395229540353,60.0635523254179)) ;
#8597 = CARTESIAN_POINT('Ctrl Pts',(-8.80490372629695,56.9553077214544,59.3921412545655)) ;
#8598 = CARTESIAN_POINT('Ctrl Pts',(-7.21100071989772,57.5027528833965,58.415849551118)) ;
#8599 = CARTESIAN_POINT('Ctrl Pts',(-6.35541866395493,57.7356392971192,58.0938755668734)) ;
#8600 = CARTESIAN_POINT('Ctrl Pts',(-4.79055478616098,58.0583687617078,57.8368826753342)) ;
#8601 = CARTESIAN_POINT('Ctrl Pts',(-4.11027061379133,58.1679507457142,57.8232388884774)) ;
#8602 = CARTESIAN_POINT('Ctrl Pts',(-2.8560896867665,58.3023925284601,57.9829957173458)) ;
#8603 = CARTESIAN_POINT('Ctrl Pts',(-2.28720555794782,58.3364158763933,58.1289673129034)) ;
#8604 = CARTESIAN_POINT('Ctrl Pts',(-1.74213662306824,58.3353824278239,58.3447753707129)) ;
#8605 = CARTESIAN_POINT('Ctrl Pts',(-4.7791282454143,45.3830585852922,88.8758193913844)) ;
#8606 = CARTESIAN_POINT('Ctrl Pts',(-5.73399192312948,45.9804850758286,87.569427889715)) ;
#8607 = CARTESIAN_POINT('Ctrl Pts',(-6.56424371575999,46.5779115664506,86.1805055162587)) ;
#8608 = CARTESIAN_POINT('Ctrl Pts',(-7.39449548054943,47.1753380370388,84.7915831893776)) ;
#8609 = CARTESIAN_POINT('Ctrl Pts',(-8.09305195315626,47.772764507627,83.3319797920042)) ;
#8610 = CARTESIAN_POINT('Ctrl Pts',(-8.79160842576309,48.3701909782153,81.8723763946309)) ;
#8611 = CARTESIAN_POINT('Ctrl Pts',(-9.35250976866712,48.9676174488035,80.35454474831)) ;
#8612 = CARTESIAN_POINT('Ctrl Pts',(-9.91341111157114,49.5650439193917,78.836713101989)) ;
#8613 = CARTESIAN_POINT('Ctrl Pts',(-10.331871912283,50.16247038998,77.2736028111546)) ;
#8614 = CARTESIAN_POINT('Ctrl Pts',(-10.7503327129948,50.7598968605682,75.7104925203202)) ;
#8615 = CARTESIAN_POINT('Ctrl Pts',(-11.0227828115078,51.3573233311564,74.1154394908365)) ;
#8616 = CARTESIAN_POINT('Ctrl Pts',(-11.2952329100208,51.9547498017447,72.5203864613528)) ;
#8617 = CARTESIAN_POINT('Ctrl Pts',(-11.4193478581578,52.5521762723329,70.9069991232676)) ;
#8618 = CARTESIAN_POINT('Ctrl Pts',(-11.5434628062947,53.1496027429211,69.2936117851824)) ;
#8619 = CARTESIAN_POINT('Ctrl Pts',(-11.5181836990798,53.7470292135094,67.6756549903998)) ;
#8620 = CARTESIAN_POINT('Ctrl Pts',(-11.4929045918648,54.3444556840976,66.0576981956171)) ;
#8621 = CARTESIAN_POINT('Ctrl Pts',(-11.3184471017276,54.9418821546858,64.4489757810347)) ;
#8622 = CARTESIAN_POINT('Ctrl Pts',(-11.1439896115904,55.5393086252741,62.8402533664523)) ;
#8623 = CARTESIAN_POINT('Ctrl Pts',(-10.8218421483247,56.1367350958623,61.2544903844918)) ;
#8624 = CARTESIAN_POINT('Ctrl Pts',(-10.499694685059,56.7341615664506,59.6687274025313)) ;
#8625 = CARTESIAN_POINT('Ctrl Pts',(-10.0326056972355,57.3315880370388,58.1194530238305)) ;
#8626 = CARTESIAN_POINT('Ctrl Pts',(-9.62163662282806,57.8572347768351,56.7563212137985)) ;
#8627 = CARTESIAN_POINT('Ctrl Pts',(-9.10130960571656,58.3831186720347,55.4310726684666)) ;
#8628 = CARTESIAN_POINT('Ctrl Pts',(17.4688390970673,45.3830585852922,72.7117248502237)) ;
#8629 = CARTESIAN_POINT('Ctrl Pts',(17.2612866360714,45.9804850758286,72.4339189895196)) ;
#8630 = CARTESIAN_POINT('Ctrl Pts',(17.0802522492153,46.5779115664506,72.1381476740026)) ;
#8631 = CARTESIAN_POINT('Ctrl Pts',(16.8992178684299,47.1753380370388,71.8423763684038)) ;
#8632 = CARTESIAN_POINT('Ctrl Pts',(16.7462460815413,47.772764507627,71.5311630257302)) ;
#8633 = CARTESIAN_POINT('Ctrl Pts',(16.5932742946527,48.3701909782152,71.2199496830565)) ;
#8634 = CARTESIAN_POINT('Ctrl Pts',(16.4696702030105,48.9676174488035,70.8959494658169)) ;
#8635 = CARTESIAN_POINT('Ctrl Pts',(16.3460661113682,49.5650439193917,70.5719492485774)) ;
#8636 = CARTESIAN_POINT('Ctrl Pts',(16.2528842615005,50.16247038998,70.2379264123862)) ;
#8637 = CARTESIAN_POINT('Ctrl Pts',(16.1597024116328,50.7598968605682,69.9039035761949)) ;
#8638 = CARTESIAN_POINT('Ctrl Pts',(16.0977377982279,51.3573233311564,69.5627078861173)) ;
#8639 = CARTESIAN_POINT('Ctrl Pts',(16.0357731848229,51.9547498017447,69.2215121960397)) ;
#8640 = CARTESIAN_POINT('Ctrl Pts',(16.005554468114,52.5521762723329,68.8760546134011)) ;
#8641 = CARTESIAN_POINT('Ctrl Pts',(15.9753357514052,53.1496027429211,68.5305970307626)) ;
#8642 = CARTESIAN_POINT('Ctrl Pts',(15.9771207468286,53.7470292135094,68.1838248778533)) ;
#8643 = CARTESIAN_POINT('Ctrl Pts',(15.9789057422521,54.3444556840976,67.837052724944)) ;
#8644 = CARTESIAN_POINT('Ctrl Pts',(16.0126792208562,54.9418821546858,67.4919245395043)) ;
#8645 = CARTESIAN_POINT('Ctrl Pts',(16.0464526994604,55.5393086252741,67.1467963540644)) ;
#8646 = CARTESIAN_POINT('Ctrl Pts',(16.111926517834,56.1367350958623,66.8062566480835)) ;
#8647 = CARTESIAN_POINT('Ctrl Pts',(16.1774003362076,56.7341615664506,66.4657169421026)) ;
#8648 = CARTESIAN_POINT('Ctrl Pts',(16.2740158948177,57.3315880370388,66.1326710802811)) ;
#8649 = CARTESIAN_POINT('Ctrl Pts',(16.3590232654268,57.8572347768351,65.8396400880374)) ;
#8650 = CARTESIAN_POINT('Ctrl Pts',(16.4675502256468,58.3831186720347,65.5544816857789)) ;
#8651 = CARTESIAN_POINT('',(16.1930072121277,58.3830537363184,65.4457829320825)) ;
#8652 = CARTESIAN_POINT('Ctrl Pts',(17.2299597049927,45.3830674541111,72.8852989434337)) ;
#8653 = CARTESIAN_POINT('Ctrl Pts',(17.2238785641997,45.3999249614351,72.8771508356198)) ;
#8654 = CARTESIAN_POINT('Ctrl Pts',(17.217728287818,45.4170195560986,72.8688763511221)) ;
#8655 = CARTESIAN_POINT('Ctrl Pts',(17.2055481051456,45.4509660823354,72.8524212486401)) ;
#8656 = CARTESIAN_POINT('Ctrl Pts',(17.1994751008465,45.467937485669,72.844182883773)) ;
#8657 = CARTESIAN_POINT('Ctrl Pts',(17.1813073904012,45.5188462146265,72.8194355027519)) ;
#8658 = CARTESIAN_POINT('Ctrl Pts',(17.1692639864156,45.5527780591987,72.802894200399)) ;
#8659 = CARTESIAN_POINT('Ctrl Pts',(17.1333393268993,45.6545524513436,72.7531423773599)) ;
#8660 = CARTESIAN_POINT('Ctrl Pts',(17.1096636365158,45.7223738576061,72.719803931897)) ;
#8661 = CARTESIAN_POINT('Ctrl Pts',(17.0567938513938,45.8755455989764,72.644103518881)) ;
#8662 = CARTESIAN_POINT('Ctrl Pts',(17.0277600220691,45.960883422686,72.601642091708)) ;
#8663 = CARTESIAN_POINT('Ctrl Pts',(16.982348309643,46.0963466756233,72.5337991217255)) ;
#8664 = CARTESIAN_POINT('Ctrl Pts',(16.9656789302262,46.1464973799211,72.5085794918992)) ;
#8665 = CARTESIAN_POINT('Ctrl Pts',(16.8728578632745,46.4282028809683,72.3663567523871)) ;
#8666 = CARTESIAN_POINT('Ctrl Pts',(16.7997590040171,46.6594344485583,72.2474911456601)) ;
#8667 = CARTESIAN_POINT('Ctrl Pts',(16.7181710871407,46.9296827699028,72.106488131638)) ;
#8668 = CARTESIAN_POINT('Ctrl Pts',(16.7064567745732,46.9687950424159,72.0860296825146)) ;
#8669 = CARTESIAN_POINT('Ctrl Pts',(16.6229150124267,47.2499758749389,71.9385824666865)) ;
#8670 = CARTESIAN_POINT('Ctrl Pts',(16.5546379309754,47.4918541916704,71.8097732580192)) ;
#8671 = CARTESIAN_POINT('Ctrl Pts',(16.4148961706487,48.0143150857792,71.527290243484)) ;
#8672 = CARTESIAN_POINT('Ctrl Pts',(16.3447756772163,48.2952954282258,71.3730820149661)) ;
#8673 = CARTESIAN_POINT('Ctrl Pts',(16.2758263325691,48.5931204307081,71.2073431067649)) ;
#8674 = CARTESIAN_POINT('Ctrl Pts',(16.2719090608717,48.6101204742725,71.1978741916928)) ;
#8675 = CARTESIAN_POINT('Ctrl Pts',(16.2074835803316,48.8910362150329,71.0412691919266)) ;
#8676 = CARTESIAN_POINT('Ctrl Pts',(16.1514139834133,49.1549226796743,70.8921635290642)) ;
#8677 = CARTESIAN_POINT('Ctrl Pts',(16.0988300543287,49.4249376060053,70.7381567568313)) ;
#8678 = CARTESIAN_POINT('Ctrl Pts',(16.0976904314877,49.4308011237537,70.7348116267408)) ;
#8679 = CARTESIAN_POINT('Ctrl Pts',(16.0441775069865,49.7066812295575,70.5773852479501)) ;
#8680 = CARTESIAN_POINT('Ctrl Pts',(15.9965787678505,49.9768666464287,70.4215354066132)) ;
#8681 = CARTESIAN_POINT('Ctrl Pts',(15.9530134055317,50.2527043291671,70.2609862544005)) ;
#8682 = CARTESIAN_POINT('Ctrl Pts',(15.9521693841446,50.2580605419637,70.2578681606108)) ;
#8683 = CARTESIAN_POINT('Ctrl Pts',(15.9096417772101,50.5285623062336,70.1003690587478)) ;
#8684 = CARTESIAN_POINT('Ctrl Pts',(15.8726896593404,50.794089282034,69.9446678031123)) ;
#8685 = CARTESIAN_POINT('Ctrl Pts',(15.8384772278282,51.0767673302898,69.7777340824964)) ;
#8686 = CARTESIAN_POINT('Ctrl Pts',(15.8364699928302,51.0935097128496,69.7678425985647)) ;
#8687 = CARTESIAN_POINT('Ctrl Pts',(15.817692972988,51.2516332986708,69.6743810453064)) ;
#8688 = CARTESIAN_POINT('Ctrl Pts',(15.8022442313088,51.3931664825854,69.5903727637932)) ;
#8689 = CARTESIAN_POINT('Ctrl Pts',(15.7769449397264,51.6479675595878,69.4388316402636)) ;
#8690 = CARTESIAN_POINT('Ctrl Pts',(15.7665891159126,51.7612319406874,69.3713494162665)) ;
#8691 = CARTESIAN_POINT('Ctrl Pts',(15.754768741742,51.9026374456281,69.286952649771)) ;
#8692 = CARTESIAN_POINT('Ctrl Pts',(15.7524687953592,51.930809108512,69.2701312609705)) ;
#8693 = CARTESIAN_POINT('Ctrl Pts',(15.7276918330122,52.2417252333189,69.0844011692014)) ;
#8694 = CARTESIAN_POINT('Ctrl Pts',(15.7107036256911,52.5241195492542,68.9147995558063)) ;
#8695 = CARTESIAN_POINT('Ctrl Pts',(15.6899375671172,53.0381974993431,68.6055750241504)) ;
#8696 = CARTESIAN_POINT('Ctrl Pts',(15.6843270313333,53.2697333986809,68.4661514431976)) ;
#8697 = CARTESIAN_POINT('Ctrl Pts',(15.6820512791615,53.5522259966907,68.2958578051499)) ;
#8698 = CARTESIAN_POINT('Ctrl Pts',(15.6818222797127,53.6031771340228,68.2651358129833)) ;
#8699 = CARTESIAN_POINT('Ctrl Pts',(15.6815693026304,53.8742457621066,68.1016504539459)) ;
#8700 = CARTESIAN_POINT('Ctrl Pts',(15.6847597300816,54.094546305059,67.9688338872412)) ;
#8701 = CARTESIAN_POINT('Ctrl Pts',(15.6932080011421,54.3774106831915,67.7985459458968)) ;
#8702 = CARTESIAN_POINT('Ctrl Pts',(15.6953459101383,54.4398806254195,67.7609537303392)) ;
#8703 = CARTESIAN_POINT('Ctrl Pts',(15.7058225897779,54.7114321392936,67.597625057857)) ;
#8704 = CARTESIAN_POINT('Ctrl Pts',(15.7169580443123,54.9205828276717,67.4719123017497)) ;
#8705 = CARTESIAN_POINT('Ctrl Pts',(15.7361100705114,55.203368432956,67.3024736213794)) ;
#8706 = CARTESIAN_POINT('Ctrl Pts',(15.7414913380932,55.2772338818112,67.25826442482)) ;
#8707 = CARTESIAN_POINT('Ctrl Pts',(15.7626401209462,55.5485088102171,67.096135261554)) ;
#8708 = CARTESIAN_POINT('Ctrl Pts',(15.7807154494597,55.7457837763595,66.9785911073384)) ;
#8709 = CARTESIAN_POINT('Ctrl Pts',(15.8104451798875,56.028258890474,66.8108962000672)) ;
#8710 = CARTESIAN_POINT('Ctrl Pts',(15.8199180013933,56.1134884206094,66.7603789490545)) ;
#8711 = CARTESIAN_POINT('Ctrl Pts',(15.8516265286932,56.3844426291125,66.6000522177058)) ;
#8712 = CARTESIAN_POINT('Ctrl Pts',(15.8757029701572,56.5701302611215,66.4907446067644)) ;
#8713 = CARTESIAN_POINT('Ctrl Pts',(15.9159005740361,56.8526653482992,66.3252858477751)) ;
#8714 = CARTESIAN_POINT('Ctrl Pts',(15.9303104866897,56.9494716030786,66.2687475535247)) ;
#8715 = CARTESIAN_POINT('Ctrl Pts',(15.97242663624,57.2204413601181,66.1109211838358)) ;
#8716 = CARTESIAN_POINT('Ctrl Pts',(16.0015712084872,57.3946576755328,66.0099460011525)) ;
#8717 = CARTESIAN_POINT('Ctrl Pts',(16.052156096611,57.6774250653639,65.847114625726)) ;
#8718 = CARTESIAN_POINT('Ctrl Pts',(16.0723519015129,57.7859396412651,65.7848796065074)) ;
#8719 = CARTESIAN_POINT('Ctrl Pts',(16.0985692319185,57.9216227418852,65.7074259475211)) ;
#8720 = CARTESIAN_POINT('Ctrl Pts',(16.1038558615345,57.9487278912594,65.6919680890366)) ;
#8721 = CARTESIAN_POINT('Ctrl Pts',(16.1225472414256,58.0436810159813,65.6378716204347)) ;
#8722 = CARTESIAN_POINT('Ctrl Pts',(16.1362123557029,58.1115399743054,65.5993088847567)) ;
#8723 = CARTESIAN_POINT('Ctrl Pts',(16.1571689589409,58.213348452282,65.5416158561056)) ;
#8724 = CARTESIAN_POINT('Ctrl Pts',(16.1642303660134,58.2472850649057,65.5224116540639)) ;
#8725 = CARTESIAN_POINT('Ctrl Pts',(16.1749370090524,58.2981973836577,65.4936437723222)) ;
#8726 = CARTESIAN_POINT('Ctrl Pts',(16.1785249790529,58.3151693899102,65.4840608820805)) ;
#8727 = CARTESIAN_POINT('Ctrl Pts',(16.1831146844042,58.3367668565652,65.4718755710812)) ;
#8728 = CARTESIAN_POINT('Ctrl Pts',(16.1841006559929,58.3413999128708,65.4692621364033)) ;
#8729 = CARTESIAN_POINT('Ctrl Pts',(16.1877259353632,58.3584108602044,65.4596685309343)) ;
#8730 = CARTESIAN_POINT('Ctrl Pts',(16.1903757616756,58.3707975233394,65.4526867860696)) ;
#8731 = CARTESIAN_POINT('Ctrl Pts',(16.193006791085,58.3830508753327,65.4457840449521)) ;
#8732 = CARTESIAN_POINT('',(-1.74213662306821,58.3831162793798,58.3447753707129)) ;
#8733 = CARTESIAN_POINT('Ctrl Pts',(16.193000981218,58.3830900980199,65.4457986821614)) ;
#8734 = CARTESIAN_POINT('Ctrl Pts',(13.2038113796415,58.383105259385,64.2622947965787)) ;
#8735 = CARTESIAN_POINT('Ctrl Pts',(10.214621778017,58.3831073991803,63.078790910977)) ;
#8736 = CARTESIAN_POINT('Ctrl Pts',(4.2362422666582,58.3831134572109,60.7117830177842)) ;
#8737 = CARTESIAN_POINT('Ctrl Pts',(1.24705235690671,58.3831150235133,59.5282790101862)) ;
#8738 = CARTESIAN_POINT('Ctrl Pts',(-1.7421375528447,58.3831162793802,58.3447750025884)) ;
#8739 = CARTESIAN_POINT('',(-11.2681471610183,55.1047242171091,64.0109093285607)) ;
#8740 = CARTESIAN_POINT('Ctrl Pts',(-1.74213662306821,58.3831162793798,58.3447753707129)) ;
#8741 = CARTESIAN_POINT('Ctrl Pts',(-2.29047317474531,58.3831165097558,58.1276735718927)) ;
#8742 = CARTESIAN_POINT('Ctrl Pts',(-2.86285096802688,58.3477204630489,57.9812725503403)) ;
#8743 = CARTESIAN_POINT('Ctrl Pts',(-4.12531944509307,58.2097834099593,57.8223467259657)) ;
#8744 = CARTESIAN_POINT('Ctrl Pts',(-4.8102892656691,58.0979492508202,57.8377999156764)) ;
#8745 = CARTESIAN_POINT('Ctrl Pts',(-6.37924732927157,57.7707079403455,58.1010309533822)) ;
#8746 = CARTESIAN_POINT('Ctrl Pts',(-7.23417879357875,57.5360203747158,58.426251502882)) ;
#8747 = CARTESIAN_POINT('Ctrl Pts',(-8.82516552869592,56.9856760363639,59.4087857781323)) ;
#8748 = CARTESIAN_POINT('Ctrl Pts',(-9.53107642063704,56.668734645817,60.0831182465607)) ;
#8749 = CARTESIAN_POINT('Ctrl Pts',(-10.4108790833113,56.1294194252976,61.3553806219125)) ;
#8750 = CARTESIAN_POINT('Ctrl Pts',(-10.6821762328728,55.9194277706208,61.8779177589046)) ;
#8751 = CARTESIAN_POINT('Ctrl Pts',(-11.0740895432526,55.5068627643851,62.9384006699818)) ;
#8752 = CARTESIAN_POINT('Ctrl Pts',(-11.2025958471988,55.3059552090325,63.4700991792931)) ;
#8753 = CARTESIAN_POINT('Ctrl Pts',(-11.2681471610183,55.104724217109,64.0109093285607)) ;
#8754 = CARTESIAN_POINT('',(-9.03444461093391,48.6398835186857,81.1828053420911)) ;
#8755 = CARTESIAN_POINT('Ctrl Pts',(-9.03444461093391,48.6398835186857,81.1828053420911)) ;
#8756 = CARTESIAN_POINT('Ctrl Pts',(-9.19872655925457,48.8038201453524,80.7706908861205)) ;
#8757 = CARTESIAN_POINT('Ctrl Pts',(-9.35250971390351,48.9676174488035,80.3545447282502)) ;
#8758 = CARTESIAN_POINT('Ctrl Pts',(-9.91341105588012,49.5650439193917,78.8367130844612)) ;
#8759 = CARTESIAN_POINT('Ctrl Pts',(-10.3318718559021,50.16247038998,77.2736027962334)) ;
#8760 = CARTESIAN_POINT('Ctrl Pts',(-10.750332655924,50.7598968605682,75.7104925080056)) ;
#8761 = CARTESIAN_POINT('Ctrl Pts',(-11.0227827539907,51.3573233311564,74.1154394811811)) ;
#8762 = CARTESIAN_POINT('Ctrl Pts',(-11.2952328520573,51.9547498017447,72.5203864543566)) ;
#8763 = CARTESIAN_POINT('Ctrl Pts',(-11.4193477999951,52.5521762723329,70.9069991189604)) ;
#8764 = CARTESIAN_POINT('Ctrl Pts',(-11.5434627479329,53.1496027429211,69.2936117835642)) ;
#8765 = CARTESIAN_POINT('Ctrl Pts',(-11.5181836407678,53.7470292135094,67.6756549914775)) ;
#8766 = CARTESIAN_POINT('Ctrl Pts',(-11.4929045336027,54.3444556840976,66.0576981993908)) ;
#8767 = CARTESIAN_POINT('Ctrl Pts',(-11.3184470437638,54.9418821546858,64.4489757874882)) ;
#8768 = CARTESIAN_POINT('Ctrl Pts',(-11.2946768606995,55.0232827101246,64.2297841307363)) ;
#8769 = CARTESIAN_POINT('Ctrl Pts',(-11.2681471610183,55.1047242171091,64.0109093285607)) ;
#8770 = CARTESIAN_POINT('Ctrl Pts',(-9.03444461093392,48.6398835186858,81.1828053420911)) ;
#8771 = CARTESIAN_POINT('Ctrl Pts',(-8.83397598669229,48.4398362807108,81.6856969796876)) ;
#8772 = CARTESIAN_POINT('Ctrl Pts',(-8.57568233556347,48.2402512214434,82.1640409953046)) ;
#8773 = CARTESIAN_POINT('Ctrl Pts',(-7.93146167760747,47.8311034847343,83.0832927130734)) ;
#8774 = CARTESIAN_POINT('Ctrl Pts',(-7.53982375225014,47.6231197022401,83.5164066873636)) ;
#8775 = CARTESIAN_POINT('Ctrl Pts',(-6.37128043545755,47.08626813226,84.5219283426251)) ;
#8776 = CARTESIAN_POINT('Ctrl Pts',(-5.51827317218396,46.770327077101,84.9961775434417)) ;
#8777 = CARTESIAN_POINT('Ctrl Pts',(-3.73052572361336,46.2216257312613,85.5454708941863)) ;
#8778 = CARTESIAN_POINT('Ctrl Pts',(-2.82130999507985,45.9879058539332,85.6443247921444)) ;
#8779 = CARTESIAN_POINT('Ctrl Pts',(-1.24213321159846,45.6640068779433,85.5034836180374)) ;
#8780 = CARTESIAN_POINT('Ctrl Pts',(-0.580849897547363,45.5539383973837,85.347630943253)) ;
#8781 = CARTESIAN_POINT('Ctrl Pts',(0.593309673962527,45.4179657782124,84.8813839044439)) ;
#8782 = CARTESIAN_POINT('Ctrl Pts',(1.10809034600835,45.3830586252741,84.5985045791954)) ;
#8783 = CARTESIAN_POINT('Ctrl Pts',(1.58245214009828,45.3830586252741,84.2538605621281)) ;
#8784 = CARTESIAN_POINT('Origin',(-2.53204462594907,45.3822493559848,78.5907416015035)) ;
#8785 = CARTESIAN_POINT('',(-9.03444461093391,45.3822493559848,81.1828053420911)) ;
#8786 = CARTESIAN_POINT('Origin',(23.4776880157599,45.3822493559848,68.2224337400009)) ;
#8787 = CARTESIAN_POINT('',(-11.2681471610183,45.3822493559848,64.0109093285607)) ;
#8788 = CARTESIAN_POINT('Origin',(-4.31900848943611,45.3822493559848,64.8532107728907)) ;
#8789 = CARTESIAN_POINT('',(-1.74213662306825,45.3822493559848,58.3447753707129)) ;
#8790 = CARTESIAN_POINT('Origin',(16.4675440301639,45.3822493559848,65.5544979647415)) ;
#8791 = CARTESIAN_POINT('Ctrl Pts',(16.3751780994845,57.8271591849708,65.5179277057667)) ;
#8792 = CARTESIAN_POINT('Ctrl Pts',(16.375098264844,57.8726765548514,65.5178960969965)) ;
#8793 = CARTESIAN_POINT('Ctrl Pts',(16.3712357710984,57.9189555946976,65.5163668275686)) ;
#8794 = CARTESIAN_POINT('Ctrl Pts',(16.3555004313488,58.0070760904206,65.5101367658406)) ;
#8795 = CARTESIAN_POINT('Ctrl Pts',(16.343438841416,58.0511720072647,65.5053612445326)) ;
#8796 = CARTESIAN_POINT('Ctrl Pts',(16.3098321161203,58.1280396089059,65.4920554007185)) ;
#8797 = CARTESIAN_POINT('Ctrl Pts',(16.2904201996508,58.1581206861651,65.4843696792975)) ;
#8798 = CARTESIAN_POINT('Ctrl Pts',(16.257133458184,58.1912258391351,65.4711905260435)) ;
#8799 = CARTESIAN_POINT('Ctrl Pts',(16.2440370654752,58.2011509268498,65.4660052973562)) ;
#8800 = CARTESIAN_POINT('Ctrl Pts',(16.2172691776374,58.2136664809846,65.4554071408364)) ;
#8801 = CARTESIAN_POINT('Ctrl Pts',(16.2043402194456,58.2169696033444,65.4502882041693)) ;
#8802 = CARTESIAN_POINT('Ctrl Pts',(16.1909560759401,58.2172758076352,65.4449890468874)) ;
#8803 = CARTESIAN_POINT('Ctrl Pts',(16.1930011817604,58.3830247512578,65.4457987615618)) ;
#8804 = CARTESIAN_POINT('Ctrl Pts',(16.1995379570469,58.3830247228401,65.4483868539821)) ;
#8805 = CARTESIAN_POINT('Ctrl Pts',(16.2060215176076,58.3837424765203,65.450953877202)) ;
#8806 = CARTESIAN_POINT('Ctrl Pts',(16.219260687547,58.3866521091205,65.4561956353886)) ;
#8807 = CARTESIAN_POINT('Ctrl Pts',(16.2259025352896,58.3889169429325,65.4588253289371)) ;
#8808 = CARTESIAN_POINT('Ctrl Pts',(16.2470604727698,58.3985444430827,65.4672023489848)) ;
#8809 = CARTESIAN_POINT('Ctrl Pts',(16.2603412472946,58.408561171848,65.4724605795664)) ;
#8810 = CARTESIAN_POINT('Ctrl Pts',(16.2929811784212,58.4411881106263,65.4853836424906)) ;
#8811 = CARTESIAN_POINT('Ctrl Pts',(16.3116752992976,58.4701790970316,65.492785168563)) ;
#8812 = CARTESIAN_POINT('Ctrl Pts',(16.344401615182,58.5450328515258,65.5057424336322)) ;
#8813 = CARTESIAN_POINT('Ctrl Pts',(16.3561655785037,58.5884055134699,65.5104001161195)) ;
#8814 = CARTESIAN_POINT('Ctrl Pts',(16.3714864465992,58.6752768777081,65.516466076911)) ;
#8815 = CARTESIAN_POINT('Ctrl Pts',(16.3751788432793,58.7210404158283,65.5179280002559)) ;
#8816 = CARTESIAN_POINT('Ctrl Pts',(16.3751784807748,58.7660404020406,65.5179278567302)) ;
#8817 = CARTESIAN_POINT('Ctrl Pts',(16.2076436667534,58.2943663992286,65.4015964591232)) ;
#8818 = CARTESIAN_POINT('Ctrl Pts',(16.3901988775676,58.2924602039142,65.4736624527373)) ;
#8819 = CARTESIAN_POINT('Ctrl Pts',(16.4544192595841,58.191081348463,65.3183511002461)) ;
#8820 = CARTESIAN_POINT('Ctrl Pts',(16.0893935021919,57.752299968197,65.7063617193311)) ;
#8821 = CARTESIAN_POINT('Ctrl Pts',(16.2749670678282,57.7503889244133,65.7707754261454)) ;
#8822 = CARTESIAN_POINT('Ctrl Pts',(16.3326721110413,57.6489874075171,65.6127858841635)) ;
#8823 = CARTESIAN_POINT('Ctrl Pts',(15.9905079233388,57.2111033102693,66.0180958060857)) ;
#8824 = CARTESIAN_POINT('Ctrl Pts',(16.1786178839759,57.2091968025795,66.0746770851081)) ;
#8825 = CARTESIAN_POINT('Ctrl Pts',(16.2296654835751,57.1078632091335,65.9143707409572)) ;
#8826 = CARTESIAN_POINT('Ctrl Pts',(15.8720965683249,56.3997926693407,66.4926301853558)) ;
#8827 = CARTESIAN_POINT('Ctrl Pts',(16.0632571274154,56.3978864499462,66.5372862974148)) ;
#8828 = CARTESIAN_POINT('Ctrl Pts',(16.1041311822517,56.296529089974,66.3742167663536)) ;
#8829 = CARTESIAN_POINT('Ctrl Pts',(15.8375699261364,56.1295297083804,66.6521222695944)) ;
#8830 = CARTESIAN_POINT('Ctrl Pts',(16.029624201713,56.1276240321266,66.6927701563547)) ;
#8831 = CARTESIAN_POINT('Ctrl Pts',(16.0670707738748,56.0262125668428,66.528911362414)) ;
#8832 = CARTESIAN_POINT('Ctrl Pts',(15.7785876369184,55.5885108130466,66.9729859773628)) ;
#8833 = CARTESIAN_POINT('Ctrl Pts',(15.9721719553117,55.5866055506255,67.0055653548671)) ;
#8834 = CARTESIAN_POINT('Ctrl Pts',(16.0027427182606,55.485272016298,66.8402402844729)) ;
#8835 = CARTESIAN_POINT('Ctrl Pts',(15.754136645686,55.317901160646,67.1342772225888)) ;
#8836 = CARTESIAN_POINT('Ctrl Pts',(15.9483601423746,55.3159940909051,67.162802173736)) ;
#8837 = CARTESIAN_POINT('Ctrl Pts',(15.9754645077105,55.2146518759505,66.9968784550975)) ;
#8838 = CARTESIAN_POINT('Ctrl Pts',(15.7153500800329,54.7764805321647,67.4585848660779)) ;
#8839 = CARTESIAN_POINT('Ctrl Pts',(15.9106003761165,54.7745728258726,67.4789559682221)) ;
#8840 = CARTESIAN_POINT('Ctrl Pts',(15.9307246503761,54.6731104541281,67.3121111144227)) ;
#8841 = CARTESIAN_POINT('Ctrl Pts',(15.7010384513997,54.5052712784467,67.6215916940795)) ;
#8842 = CARTESIAN_POINT('Ctrl Pts',(15.896670066885,54.5033650628029,67.6378592813634)) ;
#8843 = CARTESIAN_POINT('Ctrl Pts',(15.9132990653192,54.4020271817646,67.4705583238743)) ;
#8844 = CARTESIAN_POINT('Ctrl Pts',(15.6827101205307,53.9638812711069,67.9474523132968)) ;
#8845 = CARTESIAN_POINT('Ctrl Pts',(15.8788516918128,53.9619749130852,67.9555219668616)) ;
#8846 = CARTESIAN_POINT('Ctrl Pts',(15.8884659090552,53.8606102461995,67.7876870896055)) ;
#8847 = CARTESIAN_POINT('Ctrl Pts',(15.6786640134442,53.69350032242,68.1106760287787)) ;
#8848 = CARTESIAN_POINT('Ctrl Pts',(15.8749323601421,53.691594608915,68.1146384349466)) ;
#8849 = CARTESIAN_POINT('Ctrl Pts',(15.8810307763445,53.5901950776882,67.9466591165899)) ;
#8850 = CARTESIAN_POINT('Ctrl Pts',(15.6808110138424,53.1525885953391,68.4368174081503)) ;
#8851 = CARTESIAN_POINT('Ctrl Pts',(15.8770716769607,53.1506832357684,68.4325700314882)) ;
#8852 = CARTESIAN_POINT('Ctrl Pts',(15.8761429126677,53.0493503316298,68.2644444735657)) ;
#8853 = CARTESIAN_POINT('Ctrl Pts',(15.6869930500739,52.8821999703205,68.5997058627992)) ;
#8854 = CARTESIAN_POINT('Ctrl Pts',(15.8831225594926,52.8802927777111,68.5913594125356)) ;
#8855 = CARTESIAN_POINT('Ctrl Pts',(15.8786793848031,52.7789455602561,68.4232981395322)) ;
#8856 = CARTESIAN_POINT('Ctrl Pts',(15.7095785926957,52.3415574725993,68.9251182619377)) ;
#8857 = CARTESIAN_POINT('Ctrl Pts',(15.9051911925639,52.3396495857393,68.9085807093587)) ;
#8858 = CARTESIAN_POINT('Ctrl Pts',(15.8937284189081,52.2381712237815,68.7409272439851)) ;
#8859 = CARTESIAN_POINT('Ctrl Pts',(15.7259867557631,52.070892318345,69.087548400577)) ;
#8860 = CARTESIAN_POINT('Ctrl Pts',(15.9212064002032,52.0689860211472,69.0669176150257)) ;
#8861 = CARTESIAN_POINT('Ctrl Pts',(15.9062323156006,51.9676510264301,68.899458753588)) ;
#8862 = CARTESIAN_POINT('Ctrl Pts',(15.7689707763681,51.5294526417263,69.4111229964008)) ;
#8863 = CARTESIAN_POINT('Ctrl Pts',(15.9631573413053,51.5275461441184,69.382342803655)) ;
#8864 = CARTESIAN_POINT('Ctrl Pts',(15.9411922096572,51.4261734609838,69.2156785502537)) ;
#8865 = CARTESIAN_POINT('Ctrl Pts',(15.7956084260211,51.2584285629724,69.5726116865006)) ;
#8866 = CARTESIAN_POINT('Ctrl Pts',(15.9891487491342,51.2565228090376,69.5397629590593)) ;
#8867 = CARTESIAN_POINT('Ctrl Pts',(15.9636931377913,51.1551340723535,69.3736053139055)) ;
#8868 = CARTESIAN_POINT('Ctrl Pts',(15.8588547216987,50.7168256229871,69.8929710826407)) ;
#8869 = CARTESIAN_POINT('Ctrl Pts',(16.0508488942934,50.714920164228,69.8520495815658)) ;
#8870 = CARTESIAN_POINT('Ctrl Pts',(16.0184554339797,50.6135869790189,69.6870716848916)) ;
#8871 = CARTESIAN_POINT('Ctrl Pts',(15.8954576104322,50.4462620313559,70.0519295278353)) ;
#8872 = CARTESIAN_POINT('Ctrl Pts',(16.086554844969,50.4443547062442,70.0070033433742)) ;
#8873 = CARTESIAN_POINT('Ctrl Pts',(16.0507194340179,50.3430015532915,69.8427504295619)) ;
#8874 = CARTESIAN_POINT('Ctrl Pts',(15.9785962095983,49.9056099882918,70.3674102992357)) ;
#8875 = CARTESIAN_POINT('Ctrl Pts',(16.1676517617608,49.9037019096486,70.3145334544655)) ;
#8876 = CARTESIAN_POINT('Ctrl Pts',(16.1249977677534,49.8022062837278,70.1520022424188)) ;
#8877 = CARTESIAN_POINT('Ctrl Pts',(16.0251026927125,49.6350408217638,70.5237830491593)) ;
#8878 = CARTESIAN_POINT('Ctrl Pts',(16.2130058621674,49.6331344367341,70.4669615662931)) ;
#8879 = CARTESIAN_POINT('Ctrl Pts',(16.166938943436,49.5318014383334,70.3052677497731)) ;
#8880 = CARTESIAN_POINT('Ctrl Pts',(16.1277963191435,49.0942250306986,70.8332456487283)) ;
#8881 = CARTESIAN_POINT('Ctrl Pts',(16.3131619984201,49.0923183862286,70.7686210208621)) ;
#8882 = CARTESIAN_POINT('Ctrl Pts',(16.2603856795457,48.9909365753751,70.6090205283714)) ;
#8883 = CARTESIAN_POINT('Ctrl Pts',(16.1840618356866,48.8238179925398,70.9865468887572)) ;
#8884 = CARTESIAN_POINT('Ctrl Pts',(16.3680337664969,48.8219121926559,70.9180551942438)) ;
#8885 = CARTESIAN_POINT('Ctrl Pts',(16.3119277610878,48.7205331729598,70.7595928038727)) ;
#8886 = CARTESIAN_POINT('Ctrl Pts',(16.3060990374279,48.2823982253115,71.2892898858962)) ;
#8887 = CARTESIAN_POINT('Ctrl Pts',(16.4870428135359,48.2804926625057,71.2131605180457)) ;
#8888 = CARTESIAN_POINT('Ctrl Pts',(16.4243469194233,48.1791582421864,71.0571604502067)) ;
#8889 = CARTESIAN_POINT('Ctrl Pts',(16.37190690666,48.0114576298554,71.4388408381481)) ;
#8890 = CARTESIAN_POINT('Ctrl Pts',(16.5512210931819,48.0095520695984,71.3589384370468)) ;
#8891 = CARTESIAN_POINT('Ctrl Pts',(16.4853051187392,47.908060964341,71.204368923494)) ;
#8892 = CARTESIAN_POINT('Ctrl Pts',(16.5129038822507,47.4697670852096,71.7337231132686)) ;
#8893 = CARTESIAN_POINT('Ctrl Pts',(16.6887086670034,47.4678622559189,71.6463775616732)) ;
#8894 = CARTESIAN_POINT('Ctrl Pts',(16.6163421825885,47.3665093096576,71.4946332104983)) ;
#8895 = CARTESIAN_POINT('Ctrl Pts',(16.5878839183077,47.1991192501698,71.8786404936035)) ;
#8896 = CARTESIAN_POINT('Ctrl Pts',(16.7618228296394,47.1972127705445,71.7876375575991)) ;
#8897 = CARTESIAN_POINT('Ctrl Pts',(16.6862917823392,47.0958808569866,71.6374299430126)) ;
#8898 = CARTESIAN_POINT('Ctrl Pts',(16.7467474591064,46.6582159321204,72.1634615282512)) ;
#8899 = CARTESIAN_POINT('Ctrl Pts',(16.9167319946848,46.6563091332048,72.0652670932486)) ;
#8900 = CARTESIAN_POINT('Ctrl Pts',(16.8350038471522,46.5549171221787,71.9183786668138)) ;
#8901 = CARTESIAN_POINT('Ctrl Pts',(16.8307007910212,46.3878930438422,72.3034640403305)) ;
#8902 = CARTESIAN_POINT('Ctrl Pts',(16.9985920820615,46.3859871917183,72.2017331629075)) ;
#8903 = CARTESIAN_POINT('Ctrl Pts',(16.9138021385845,46.2846172014626,72.056576034241)) ;
#8904 = CARTESIAN_POINT('Ctrl Pts',(17.0070827839767,45.8470089936314,72.5777188611197)) ;
#8905 = CARTESIAN_POINT('Ctrl Pts',(17.1705743029419,45.8451033189024,72.4690595698271)) ;
#8906 = CARTESIAN_POINT('Ctrl Pts',(17.0797814323178,45.7437666877221,72.3275569160594)) ;
#8907 = CARTESIAN_POINT('Ctrl Pts',(17.0995563707454,45.5765948766489,72.7120629137262)) ;
#8908 = CARTESIAN_POINT('Ctrl Pts',(17.2607441051786,45.5746876691147,72.6000093665917)) ;
#8909 = CARTESIAN_POINT('Ctrl Pts',(17.1670266235441,45.4732994149914,72.4604609422583)) ;
#8910 = CARTESIAN_POINT('Ctrl Pts',(17.1962999806241,45.3060601767044,72.8435636952195)) ;
#8911 = CARTESIAN_POINT('Ctrl Pts',(17.3550714514673,45.3041537286489,72.7281859629674)) ;
#8912 = CARTESIAN_POINT('Ctrl Pts',(17.2584885598876,45.2027271666488,72.5906780243875)) ;
#8913 = CARTESIAN_POINT('Ctrl Pts',(17.2968875596656,45.1993067880442,72.973657143502)) ;
#8914 = CARTESIAN_POINT('Ctrl Pts',(17.451249335316,45.2022951414426,72.855866322441)) ;
#8915 = CARTESIAN_POINT('Ctrl Pts',(17.5553932904832,45.3026470834629,72.9854606506312)) ;
#8916 = CARTESIAN_POINT('Ctrl Pts',(17.1929325562347,45.4820412744203,72.8384255376541)) ;
#8917 = CARTESIAN_POINT('Ctrl Pts',(17.3498724730783,45.4850280413069,72.7240107837351)) ;
#8918 = CARTESIAN_POINT('Ctrl Pts',(17.4511824806264,45.5853775943584,72.8558860880284)) ;
#8919 = CARTESIAN_POINT('Ctrl Pts',(17.0936474486457,45.7643410734892,72.7000748128061)) ;
#8920 = CARTESIAN_POINT('Ctrl Pts',(17.2530462868952,45.7673284499132,72.5891193657422)) ;
#8921 = CARTESIAN_POINT('Ctrl Pts',(17.3514803736145,45.8675945653398,72.7232114728561)) ;
#8922 = CARTESIAN_POINT('Ctrl Pts',(16.9046842952674,46.328018306681,72.4177729528116)) ;
#8923 = CARTESIAN_POINT('Ctrl Pts',(17.0687646573102,46.331005889118,72.3138645852439)) ;
#8924 = CARTESIAN_POINT('Ctrl Pts',(17.1612596670856,46.4312885658147,72.4521090456578)) ;
#8925 = CARTESIAN_POINT('Ctrl Pts',(16.8148839283541,46.6093355962119,72.2736303591509)) ;
#8926 = CARTESIAN_POINT('Ctrl Pts',(16.9811890146995,46.6123226913613,72.1733185766999)) ;
#8927 = CARTESIAN_POINT('Ctrl Pts',(17.070637445787,46.7126511405725,72.3135226725028)) ;
#8928 = CARTESIAN_POINT('Ctrl Pts',(16.6450769382365,47.1717937445032,71.9801663667652)) ;
#8929 = CARTESIAN_POINT('Ctrl Pts',(16.8155843847405,47.1747799487467,71.8871818339373)) ;
#8930 = CARTESIAN_POINT('Ctrl Pts',(16.898874585859,47.2750367263762,72.0311762509218)) ;
#8931 = CARTESIAN_POINT('Ctrl Pts',(16.5650865575195,47.4527838882157,71.8308984330576)) ;
#8932 = CARTESIAN_POINT('Ctrl Pts',(16.7375724992622,47.4557728130825,71.7416366037205)) ;
#8933 = CARTESIAN_POINT('Ctrl Pts',(16.8177106448256,47.5560442950795,71.8873993380807)) ;
#8934 = CARTESIAN_POINT('Ctrl Pts',(16.4149022782682,48.0142871287587,71.5273059776434)) ;
#8935 = CARTESIAN_POINT('Ctrl Pts',(16.5911042040292,48.0172777959156,71.4456128616253)) ;
#8936 = CARTESIAN_POINT('Ctrl Pts',(16.6648000440323,48.1176897428506,71.5946479830374)) ;
#8937 = CARTESIAN_POINT('Ctrl Pts',(16.3447812976334,48.2952668190988,71.3730983517084)) ;
#8938 = CARTESIAN_POINT('Ctrl Pts',(16.5227137172553,48.2982544973843,71.2952593298538)) ;
#8939 = CARTESIAN_POINT('Ctrl Pts',(16.5931940987698,48.3985111247922,71.4459383708063)) ;
#8940 = CARTESIAN_POINT('Ctrl Pts',(16.214741633037,48.8569739450496,71.0605092697478)) ;
#8941 = CARTESIAN_POINT('Ctrl Pts',(16.3958861388272,48.8599622667949,70.9904650444409)) ;
#8942 = CARTESIAN_POINT('Ctrl Pts',(16.4597477106443,48.9602706397639,71.1440347517157)) ;
#8943 = CARTESIAN_POINT('Ctrl Pts',(16.1547372811686,49.1378578224163,70.9018967081238)) ;
#8944 = CARTESIAN_POINT('Ctrl Pts',(16.3373622620764,49.1408449473386,70.8358093418605)) ;
#8945 = CARTESIAN_POINT('Ctrl Pts',(16.3978721266104,49.2411421341037,70.9907371606981)) ;
#8946 = CARTESIAN_POINT('Ctrl Pts',(16.045206308162,49.7002903801079,70.5811055636178)) ;
#8947 = CARTESIAN_POINT('Ctrl Pts',(16.2305301078175,49.7032770483596,70.523019074802)) ;
#8948 = CARTESIAN_POINT('Ctrl Pts',(16.284256690246,49.8035375139106,70.6804497323144)) ;
#8949 = CARTESIAN_POINT('Ctrl Pts',(15.9956378175181,49.9815741041282,70.4188518451987)) ;
#8950 = CARTESIAN_POINT('Ctrl Pts',(16.1821849956454,49.9845613531715,70.3648063422433)) ;
#8951 = CARTESIAN_POINT('Ctrl Pts',(16.2324502058595,50.0849543128215,70.5232979085427)) ;
#8952 = CARTESIAN_POINT('Ctrl Pts',(15.9070166158438,50.5452598054762,70.090646978502)) ;
#8953 = CARTESIAN_POINT('Ctrl Pts',(16.0957390532765,50.5482454986069,70.044788576911)) ;
#8954 = CARTESIAN_POINT('Ctrl Pts',(16.1390683728253,50.6485130930204,70.2053882479554)) ;
#8955 = CARTESIAN_POINT('Ctrl Pts',(15.8680534537747,50.8275371605423,69.9250501649938)) ;
#8956 = CARTESIAN_POINT('Ctrl Pts',(16.0577309660869,50.8305252760806,69.8833184453582)) ;
#8957 = CARTESIAN_POINT('Ctrl Pts',(16.0975469811511,50.9307809743298,70.0448322276628)) ;
#8958 = CARTESIAN_POINT('Ctrl Pts',(15.817695468004,51.2516112326466,69.6743941084036)) ;
#8959 = CARTESIAN_POINT('Ctrl Pts',(16.0086068770328,51.2545993841867,69.6389077620491)) ;
#8960 = CARTESIAN_POINT('Ctrl Pts',(16.0430917908323,51.3549223743145,69.8015738795152)) ;
#8961 = CARTESIAN_POINT('Ctrl Pts',(15.8022455195989,51.3931523912035,69.5903811628836)) ;
#8962 = CARTESIAN_POINT('Ctrl Pts',(15.9935348337152,51.3961401671646,69.5569883942883)) ;
#8963 = CARTESIAN_POINT('Ctrl Pts',(16.0262336376549,51.4964802131712,69.7200131309892)) ;
#8964 = CARTESIAN_POINT('Ctrl Pts',(15.7741453113461,51.6761627264733,69.422062782985)) ;
#8965 = CARTESIAN_POINT('Ctrl Pts',(15.9661181557686,51.6791498413111,69.3928666277847)) ;
#8966 = CARTESIAN_POINT('Ctrl Pts',(15.9952469927814,51.7794366542442,69.556597417726)) ;
#8967 = CARTESIAN_POINT('Ctrl Pts',(15.761490146833,51.8176028378204,69.3377566191795)) ;
#8968 = CARTESIAN_POINT('Ctrl Pts',(15.9537703088477,51.8205901090039,69.3106616104865)) ;
#8969 = CARTESIAN_POINT('Ctrl Pts',(15.9811083432102,51.9208634696797,69.4747085828085)) ;
#8970 = CARTESIAN_POINT('Ctrl Pts',(15.727691356137,52.2417288193164,69.0843990475119)) ;
#8971 = CARTESIAN_POINT('Ctrl Pts',(15.9207908993607,52.244716110021,69.0636171801009)) ;
#8972 = CARTESIAN_POINT('Ctrl Pts',(15.9427411584188,52.3449902631942,69.2285011527611)) ;
#8973 = CARTESIAN_POINT('Ctrl Pts',(15.7107023087123,52.5241300049526,68.9147933424545)) ;
#8974 = CARTESIAN_POINT('Ctrl Pts',(15.9042121206607,52.5271171122649,68.8982355118463)) ;
#8975 = CARTESIAN_POINT('Ctrl Pts',(15.9225483779282,52.6274614458918,69.0635205182557)) ;
#8976 = CARTESIAN_POINT('Ctrl Pts',(15.6878767651245,53.0891744812518,68.5749117700964)) ;
#8977 = CARTESIAN_POINT('Ctrl Pts',(15.881922329841,53.0921605107966,68.5668240512164)) ;
#8978 = CARTESIAN_POINT('Ctrl Pts',(15.8930266987946,53.1924181127708,68.7328008850591)) ;
#8979 = CARTESIAN_POINT('Ctrl Pts',(15.6820372968995,53.3716654702733,68.4047638003974)) ;
#8980 = CARTESIAN_POINT('Ctrl Pts',(15.8762134290656,53.3746541735213,68.4009124350081)) ;
#8981 = CARTESIAN_POINT('Ctrl Pts',(15.8836899306515,53.4749194098514,68.5670880136959)) ;
#8982 = CARTESIAN_POINT('Ctrl Pts',(15.6815112504157,53.9365848433274,68.0640528555997)) ;
#8983 = CARTESIAN_POINT('Ctrl Pts',(15.8756745974021,53.939575131127,68.0686834602829)) ;
#8984 = CARTESIAN_POINT('Ctrl Pts',(15.8758831838286,54.0399680491534,68.2349550032619)) ;
#8985 = CARTESIAN_POINT('Ctrl Pts',(15.6868397059094,54.2194050938135,67.8935619946214)) ;
#8986 = CARTESIAN_POINT('Ctrl Pts',(15.88085072629,54.2223926611942,67.9024431647425)) ;
#8987 = CARTESIAN_POINT('Ctrl Pts',(15.8774231007484,54.3226514036281,68.0687552371563)) ;
#8988 = CARTESIAN_POINT('Ctrl Pts',(15.7086729983829,54.7853172886158,67.553185729259)) ;
#8989 = CARTESIAN_POINT('Ctrl Pts',(15.9021114891387,54.7883053531188,67.5705413052623)) ;
#8990 = CARTESIAN_POINT('Ctrl Pts',(15.8914153126205,54.8886040661601,67.736521881602)) ;
#8991 = CARTESIAN_POINT('Ctrl Pts',(15.7252052959611,55.0683374452749,67.3831126794745)) ;
#8992 = CARTESIAN_POINT('Ctrl Pts',(15.9182171697501,55.0713245454019,67.404703163084)) ;
#8993 = CARTESIAN_POINT('Ctrl Pts',(15.9038874382428,55.1716304682316,67.5704054125967)) ;
#8994 = CARTESIAN_POINT('Ctrl Pts',(15.769289072919,55.6338317485951,67.0451410222993)) ;
#8995 = CARTESIAN_POINT('Ctrl Pts',(15.9611713077456,55.6368182566034,67.0751464795178)) ;
#8996 = CARTESIAN_POINT('Ctrl Pts',(15.9396114207564,55.7370765662141,67.240090940531)) ;
#8997 = CARTESIAN_POINT('Ctrl Pts',(15.7968305063234,55.9162154787387,66.8771073253589)) ;
#8998 = CARTESIAN_POINT('Ctrl Pts',(15.9880173845642,55.9192027777541,66.9112923600459)) ;
#8999 = CARTESIAN_POINT('Ctrl Pts',(15.9628724013359,56.0196099645353,67.0756434800854)) ;
#9000 = CARTESIAN_POINT('Ctrl Pts',(15.8629517303589,56.481225490452,66.542784474632)) ;
#9001 = CARTESIAN_POINT('Ctrl Pts',(16.0524570183557,56.4842111077296,66.585293753671)) ;
#9002 = CARTESIAN_POINT('Ctrl Pts',(16.0201417374786,56.5844827370484,66.7484645657872)) ;
#9003 = CARTESIAN_POINT('Ctrl Pts',(15.9014426423274,56.7637439358746,66.3769244785956)) ;
#9004 = CARTESIAN_POINT('Ctrl Pts',(16.0899742906582,56.7667319249263,66.4235600545759)) ;
#9005 = CARTESIAN_POINT('Ctrl Pts',(16.0541008627812,56.8669869420473,66.5859953376069)) ;
#9006 = CARTESIAN_POINT('Ctrl Pts',(15.9892699006111,57.3288079962382,66.0478030471487)) ;
#9007 = CARTESIAN_POINT('Ctrl Pts',(16.1755881248362,57.3317969661861,66.1026263528049)) ;
#9008 = CARTESIAN_POINT('Ctrl Pts',(16.1326652899509,57.4321309086594,66.2632966799852)) ;
#9009 = CARTESIAN_POINT('Ctrl Pts',(16.0386461895469,57.6115036703746,65.8844549210715)) ;
#9010 = CARTESIAN_POINT('Ctrl Pts',(16.2237177401031,57.6144908954445,65.9433440431311)) ;
#9011 = CARTESIAN_POINT('Ctrl Pts',(16.1772817370448,57.7147692588153,66.1030671471929)) ;
#9012 = CARTESIAN_POINT('Ctrl Pts',(16.1480173189084,58.1775332619219,65.5613413260415)) ;
#9013 = CARTESIAN_POINT('Ctrl Pts',(16.3303358670001,58.1805203783525,65.6282684666599)) ;
#9014 = CARTESIAN_POINT('Ctrl Pts',(16.2769572424907,58.2807900093283,65.7858125302268)) ;
#9015 = CARTESIAN_POINT('Ctrl Pts',(16.2080701484261,58.4605262973704,65.4014232574249)) ;
#9016 = CARTESIAN_POINT('Ctrl Pts',(16.3888822517855,58.4635120170919,65.4723277868928)) ;
#9017 = CARTESIAN_POINT('Ctrl Pts',(16.3320875218486,58.5638924134504,65.6286060519377)) ;
#9018 = CARTESIAN_POINT('Ctrl Pts',(16.2731529226733,58.7433256931628,65.2440040205795)) ;
#9019 = CARTESIAN_POINT('Ctrl Pts',(16.4523242289707,58.7463128973535,65.3188245830744)) ;
#9020 = CARTESIAN_POINT('Ctrl Pts',(16.3921137230323,58.846547398596,65.4738637287654)) ;
#9021 = CARTESIAN_POINT('Origin',(34.3408356446983,45.3830586252741,101.493960960612)) ;
#9022 = CARTESIAN_POINT('',(25.8874434877188,45.3830610445957,75.638885508351)) ;
#9023 = CARTESIAN_POINT('',(32.2277009906555,45.3830586252741,95.1522046229055)) ;
#9024 = CARTESIAN_POINT('',(25.8874396740751,45.3830586252741,75.6388867474779)) ;
#9025 = CARTESIAN_POINT('Ctrl Pts',(25.8874448759437,45.3830586252741,75.6388850572898)) ;
#9026 = CARTESIAN_POINT('Ctrl Pts',(25.8831721961058,45.3830586252741,75.6257350973774)) ;
#9027 = CARTESIAN_POINT('Ctrl Pts',(25.877335045612,45.3830586252741,75.6131877264577)) ;
#9028 = CARTESIAN_POINT('Ctrl Pts',(25.8622162570581,45.3830586252741,75.5887217865201)) ;
#9029 = CARTESIAN_POINT('Ctrl Pts',(25.8527987231294,45.3830586252741,75.5770968153146)) ;
#9030 = CARTESIAN_POINT('Ctrl Pts',(25.8226143339006,45.3830586252741,75.5477565599384)) ;
#9031 = CARTESIAN_POINT('Ctrl Pts',(25.799308805845,45.3830586252741,75.5332471960665)) ;
#9032 = CARTESIAN_POINT('Ctrl Pts',(25.7465957636447,45.3830586252741,75.5124525882851)) ;
#9033 = CARTESIAN_POINT('Ctrl Pts',(25.7172005505345,45.3830586252736,75.5070624718622)) ;
#9034 = CARTESIAN_POINT('Ctrl Pts',(25.6610381928182,45.3830586252736,75.5063308717296)) ;
#9035 = CARTESIAN_POINT('Ctrl Pts',(25.634330653479,45.3830586252741,75.5100675780367)) ;
#9036 = CARTESIAN_POINT('Ctrl Pts',(25.6087276455907,45.3830586252741,75.5175467475628)) ;
#9037 = CARTESIAN_POINT('',(25.9816821278123,45.3830674541116,75.6052810522977)) ;
#9038 = CARTESIAN_POINT('Ctrl Pts',(26.1331741609198,45.3830586252741,75.3434163707841)) ;
#9039 = CARTESIAN_POINT('Ctrl Pts',(26.108588619251,45.3830586252741,75.3525850395932)) ;
#9040 = CARTESIAN_POINT('Ctrl Pts',(26.0853132912683,45.3830586252745,75.3652945006832)) ;
#9041 = CARTESIAN_POINT('Ctrl Pts',(26.040864706517,45.3830586252745,75.3990270570443)) ;
#9042 = CARTESIAN_POINT('Ctrl Pts',(26.0203779564856,45.3830586252741,75.4208777603213)) ;
#9043 = CARTESIAN_POINT('Ctrl Pts',(25.9902687734762,45.3830586252741,75.4690276156026)) ;
#9044 = CARTESIAN_POINT('Ctrl Pts',(25.980120414945,45.3830586252741,75.4946011380552)) ;
#9045 = CARTESIAN_POINT('Ctrl Pts',(25.9733020175168,45.3830586252741,75.5359676129567)) ;
#9046 = CARTESIAN_POINT('Ctrl Pts',(25.972614510739,45.3830586252741,75.5506847426767)) ;
#9047 = CARTESIAN_POINT('Ctrl Pts',(25.97483660085,45.3830586252741,75.5789335804189)) ;
#9048 = CARTESIAN_POINT('Ctrl Pts',(25.9774754040238,45.3830586252741,75.5923171052466)) ;
#9049 = CARTESIAN_POINT('Ctrl Pts',(25.9816871705707,45.3830586252741,75.6052793419901)) ;
#9050 = CARTESIAN_POINT('',(31.9584809790255,45.3830586252741,94.000023827484)) ;
#9051 = CARTESIAN_POINT('',(31.9584809790255,45.3830586252741,94.000023827484)) ;
#9052 = CARTESIAN_POINT('Origin',(25.3010853649595,45.3830586252741,96.1631427881087)) ;
#9053 = CARTESIAN_POINT('Ctrl Pts',(25.7953201020593,45.38305024022,75.3553561083262)) ;
#9054 = CARTESIAN_POINT('Ctrl Pts',(25.465542879517,45.9804808943737,75.46250745988)) ;
#9055 = CARTESIAN_POINT('Ctrl Pts',(25.1272856995576,46.5779115664506,75.5387734998541)) ;
#9056 = CARTESIAN_POINT('Ctrl Pts',(24.7890308984242,47.1753380370388,75.61503900348)) ;
#9057 = CARTESIAN_POINT('Ctrl Pts',(24.4451821397366,47.772764507627,75.6597689563314)) ;
#9058 = CARTESIAN_POINT('Ctrl Pts',(24.101333381049,48.3701909782152,75.7044989091829)) ;
#9059 = CARTESIAN_POINT('Ctrl Pts',(23.7548242611786,48.9676174488035,75.7173116910735)) ;
#9060 = CARTESIAN_POINT('Ctrl Pts',(23.4083151413083,49.5650439193917,75.7301244729642)) ;
#9061 = CARTESIAN_POINT('Ctrl Pts',(23.0621019538903,50.16247038998,75.7109107697566)) ;
#9062 = CARTESIAN_POINT('Ctrl Pts',(22.7158887664722,50.7598968605682,75.6916970665491)) ;
#9063 = CARTESIAN_POINT('Ctrl Pts',(22.3729252803503,51.3573233311564,75.6406208027845)) ;
#9064 = CARTESIAN_POINT('Ctrl Pts',(22.0299617942283,51.9547498017447,75.5895445390199)) ;
#9065 = CARTESIAN_POINT('Ctrl Pts',(21.6931740529404,52.5521762723329,75.5070414793717)) ;
#9066 = CARTESIAN_POINT('Ctrl Pts',(21.3563863116525,53.1496027429211,75.4245384197236)) ;
#9067 = CARTESIAN_POINT('Ctrl Pts',(21.0286476694594,53.7470292135094,75.311312451207)) ;
#9068 = CARTESIAN_POINT('Ctrl Pts',(20.7009090272663,54.3444556840976,75.1980864826905)) ;
#9069 = CARTESIAN_POINT('Ctrl Pts',(20.3850156347058,54.9418821546858,75.0551036093466)) ;
#9070 = CARTESIAN_POINT('Ctrl Pts',(20.0691222421452,55.5393086252741,74.9121207360026)) ;
#9071 = CARTESIAN_POINT('Ctrl Pts',(19.7677691902617,56.1367350958623,74.7406008372924)) ;
#9072 = CARTESIAN_POINT('Ctrl Pts',(19.4664161383782,56.7341615664506,74.5690809385821)) ;
#9073 = CARTESIAN_POINT('Ctrl Pts',(19.1821744651562,57.3315880370388,74.3704873618051)) ;
#9074 = CARTESIAN_POINT('Ctrl Pts',(18.9320941337912,57.8572133193466,74.1957615838275)) ;
#9075 = CARTESIAN_POINT('Ctrl Pts',(18.6970309148446,58.3830758086166,74.0013019409091)) ;
#9076 = CARTESIAN_POINT('Ctrl Pts',(34.2933044184902,45.38305024022,101.509404792186)) ;
#9077 = CARTESIAN_POINT('Ctrl Pts',(32.7543440466264,45.9804808943737,102.00944443277)) ;
#9078 = CARTESIAN_POINT('Ctrl Pts',(31.1758105401488,46.5779115664505,102.365352619316)) ;
#9079 = CARTESIAN_POINT('Ctrl Pts',(29.5972881348596,47.1753380370388,102.721258302903)) ;
#9080 = CARTESIAN_POINT('Ctrl Pts',(27.9926605943175,47.772764507627,102.929998082877)) ;
#9081 = CARTESIAN_POINT('Ctrl Pts',(26.3880330537754,48.3701909782152,103.13873786285)) ;
#9082 = CARTESIAN_POINT('Ctrl Pts',(24.7709904943805,48.9676174488035,103.198530845007)) ;
#9083 = CARTESIAN_POINT('Ctrl Pts',(23.1539479349856,49.5650439193917,103.258323827163)) ;
#9084 = CARTESIAN_POINT('Ctrl Pts',(21.5382863937015,50.16247038998,103.168659878861)) ;
#9085 = CARTESIAN_POINT('Ctrl Pts',(19.9226248524173,50.7598968605682,103.078995930559)) ;
#9086 = CARTESIAN_POINT('Ctrl Pts',(18.3221285838481,51.3573233311564,102.840640032991)) ;
#9087 = CARTESIAN_POINT('Ctrl Pts',(16.7216323152788,51.9547498017447,102.602284135423)) ;
#9088 = CARTESIAN_POINT('Ctrl Pts',(15.1499561892687,52.5521762723329,102.217269857065)) ;
#9089 = CARTESIAN_POINT('Ctrl Pts',(13.5782800632586,53.1496027429211,101.832255578707)) ;
#9090 = CARTESIAN_POINT('Ctrl Pts',(12.0488330663575,53.7470292135094,101.30386772563)) ;
#9091 = CARTESIAN_POINT('Ctrl Pts',(10.5193860694563,54.3444556840976,100.775479872552)) ;
#9092 = CARTESIAN_POINT('Ctrl Pts',(9.04521690417374,54.9418821546858,100.108226463614)) ;
#9093 = CARTESIAN_POINT('Ctrl Pts',(7.57104773889119,55.5393086252741,99.4409730546758)) ;
#9094 = CARTESIAN_POINT('Ctrl Pts',(6.16473349676808,56.1367350958623,98.6405468606946)) ;
#9095 = CARTESIAN_POINT('Ctrl Pts',(4.75841925464496,56.7341615664505,97.8401206667133)) ;
#9096 = CARTESIAN_POINT('Ctrl Pts',(3.43195811294263,57.3315880370388,96.9133506417539)) ;
#9097 = CARTESIAN_POINT('Ctrl Pts',(2.26491656657273,57.8572133193466,96.0979636778584)) ;
#9098 = CARTESIAN_POINT('Ctrl Pts',(1.16795487815523,58.3830758086166,95.1904853442392)) ;
#9099 = CARTESIAN_POINT('',(6.29012224935737,58.3353824278239,89.1555480018396)) ;
#9100 = CARTESIAN_POINT('',(18.5844591889196,58.2172712656977,74.2942518441039)) ;
#9101 = CARTESIAN_POINT('Ctrl Pts',(6.2901222493574,58.3353824278239,89.1555480018396)) ;
#9102 = CARTESIAN_POINT('Ctrl Pts',(7.9341551303245,58.3308357090662,87.1682536299972)) ;
#9103 = CARTESIAN_POINT('Ctrl Pts',(9.7767093026726,58.3244410141138,84.9409882395581)) ;
#9104 = CARTESIAN_POINT('Ctrl Pts',(12.9422976968674,58.3066351840462,81.1144492012072)) ;
#9105 = CARTESIAN_POINT('Ctrl Pts',(16.4192438916362,58.2895264446024,76.9115432349964)) ;
#9106 = CARTESIAN_POINT('Ctrl Pts',(18.5844570548379,58.2172696107887,74.2942501243266)) ;
#9107 = CARTESIAN_POINT('Ctrl Pts',(18.5844591889196,58.2172712656977,74.2942518441039)) ;
#9108 = CARTESIAN_POINT('Ctrl Pts',(18.7101800665396,57.9495340002374,74.3955675893354)) ;
#9109 = CARTESIAN_POINT('Ctrl Pts',(18.839000643377,57.6819084045899,74.4929334901453)) ;
#9110 = CARTESIAN_POINT('Ctrl Pts',(18.9705754040965,57.4145313636573,74.5861224918267)) ;
#9111 = CARTESIAN_POINT('Ctrl Pts',(19.0927155785282,57.1663266301663,74.6726293633439)) ;
#9112 = CARTESIAN_POINT('Ctrl Pts',(19.2172631286827,56.9182638872732,74.7555641589253)) ;
#9113 = CARTESIAN_POINT('Ctrl Pts',(19.3440508641358,56.6702295478716,74.8348238368534)) ;
#9114 = CARTESIAN_POINT('Ctrl Pts',(19.3538444462716,56.651070402338,74.8409461653505)) ;
#9115 = CARTESIAN_POINT('Ctrl Pts',(19.3636520874551,56.6319118940955,74.8470470101628)) ;
#9116 = CARTESIAN_POINT('Ctrl Pts',(19.3734736865329,56.6127538456681,74.8531263066697)) ;
#9117 = CARTESIAN_POINT('Ctrl Pts',(19.5022865921394,56.361490903236,74.9328579105444)) ;
#9118 = CARTESIAN_POINT('Ctrl Pts',(19.6334867409694,56.1103350670491,75.0088728946902)) ;
#9119 = CARTESIAN_POINT('Ctrl Pts',(19.7667733325224,55.8590202585562,75.0809886233964)) ;
#9120 = CARTESIAN_POINT('Ctrl Pts',(19.7752158365134,55.8431017310511,75.0855565046838)) ;
#9121 = CARTESIAN_POINT('Ctrl Pts',(19.7836664501678,55.8271830724926,75.0901086434416)) ;
#9122 = CARTESIAN_POINT('Ctrl Pts',(19.7921251649139,55.8112643008986,75.0946450326021)) ;
#9123 = CARTESIAN_POINT('Ctrl Pts',(19.927388862856,55.5567064895584,75.1671866410578)) ;
#9124 = CARTESIAN_POINT('Ctrl Pts',(20.0647904015071,55.3019957844152,75.2357353524665)) ;
#9125 = CARTESIAN_POINT('Ctrl Pts',(20.2043059526064,55.0471908391173,75.3002604585485)) ;
#9126 = CARTESIAN_POINT('Ctrl Pts',(20.2112552757719,55.034498906963,75.303474478856)) ;
#9127 = CARTESIAN_POINT('Ctrl Pts',(20.2182098394889,55.0218058655745,75.3066784613102)) ;
#9128 = CARTESIAN_POINT('Ctrl Pts',(20.2251695507038,55.0091118266698,75.3098723681775)) ;
#9129 = CARTESIAN_POINT('Ctrl Pts',(20.3666875736652,54.7509925981976,75.3748169285795)) ;
#9130 = CARTESIAN_POINT('Ctrl Pts',(20.510254348456,54.4926055130936,75.4355599269685)) ;
#9131 = CARTESIAN_POINT('Ctrl Pts',(20.6552605035336,54.2345762733044,75.4918603128164)) ;
#9132 = CARTESIAN_POINT('Ctrl Pts',(20.6605536210439,54.2251575070005,75.4939154294286)) ;
#9133 = CARTESIAN_POINT('Ctrl Pts',(20.6658490728384,54.2157389752755,75.4959647949841)) ;
#9134 = CARTESIAN_POINT('Ctrl Pts',(20.6711468481269,54.2063206495464,75.498008405768)) ;
#9135 = CARTESIAN_POINT('Ctrl Pts',(20.8181077649379,53.9450551732693,75.5546984120534)) ;
#9136 = CARTESIAN_POINT('Ctrl Pts',(20.9667953261445,53.6840579939653,75.6069349668757)) ;
#9137 = CARTESIAN_POINT('Ctrl Pts',(21.1167903730235,53.4230444575826,75.6545818341298)) ;
#9138 = CARTESIAN_POINT('Ctrl Pts',(21.1203326411854,53.416880387775,75.6557070578249)) ;
#9139 = CARTESIAN_POINT('Ctrl Pts',(21.1238756222229,53.4107163827002,75.65682972301)) ;
#9140 = CARTESIAN_POINT('Ctrl Pts',(21.127419315629,53.4045524432165,75.6579498295793)) ;
#9141 = CARTESIAN_POINT('Ctrl Pts',(21.2793512822543,53.1402803009654,75.705973169749)) ;
#9142 = CARTESIAN_POINT('Ctrl Pts',(21.4326359576011,52.876053372543,75.7493072487968)) ;
#9143 = CARTESIAN_POINT('Ctrl Pts',(21.5872704788157,52.6118787196962,75.7879471921473)) ;
#9144 = CARTESIAN_POINT('Ctrl Pts',(21.7452985588166,52.341906576048,75.8274351150965)) ;
#9145 = CARTESIAN_POINT('Ctrl Pts',(21.9046488421704,52.0715787920638,75.8619872769898)) ;
#9146 = CARTESIAN_POINT('Ctrl Pts',(22.0649600027153,51.8011908422986,75.8915185741482)) ;
#9147 = CARTESIAN_POINT('Ctrl Pts',(22.0651612626675,51.8008513882913,75.8915556487189)) ;
#9148 = CARTESIAN_POINT('Ctrl Pts',(22.0653625241294,51.8005119341973,75.8915927153756)) ;
#9149 = CARTESIAN_POINT('Ctrl Pts',(22.0655637871,51.8001724800173,75.8916297741181)) ;
#9150 = CARTESIAN_POINT('Ctrl Pts',(22.2239547698191,51.5330270582815,75.9207944566424)) ;
#9151 = CARTESIAN_POINT('Ctrl Pts',(22.3836176559041,51.2655853544539,75.9451032765368)) ;
#9152 = CARTESIAN_POINT('Ctrl Pts',(22.5435526953119,50.998401550286,75.9644006663621)) ;
#9153 = CARTESIAN_POINT('Ctrl Pts',(22.5457025607775,50.9948100344075,75.9646600641283)) ;
#9154 = CARTESIAN_POINT('Ctrl Pts',(22.5478524859572,50.9912185474961,75.9649185578724)) ;
#9155 = CARTESIAN_POINT('Ctrl Pts',(22.5500024684931,50.9876270907846,75.9651761472065)) ;
#9156 = CARTESIAN_POINT('Ctrl Pts',(22.7079994706035,50.7236996475827,75.9841057626246)) ;
#9157 = CARTESIAN_POINT('Ctrl Pts',(22.8663838034903,50.4599498020535,75.9981821182529)) ;
#9158 = CARTESIAN_POINT('Ctrl Pts',(23.0251541201544,50.1963788513668,76.0074120799679)) ;
#9159 = CARTESIAN_POINT('Ctrl Pts',(23.0292590911529,50.189564283434,76.007650718562)) ;
#9160 = CARTESIAN_POINT('Ctrl Pts',(23.0333642180568,50.1827500045964,76.007886111495)) ;
#9161 = CARTESIAN_POINT('Ctrl Pts',(23.0374695044909,50.175936008737,76.0081182595862)) ;
#9162 = CARTESIAN_POINT('Ctrl Pts',(23.1943074066204,49.9156148757611,76.0169872192053)) ;
#9163 = CARTESIAN_POINT('Ctrl Pts',(23.3512376999488,49.6552611188171,76.0211072512855)) ;
#9164 = CARTESIAN_POINT('Ctrl Pts',(23.5082061089285,49.3948957256022,76.0204931855221)) ;
#9165 = CARTESIAN_POINT('Ctrl Pts',(23.5142878202418,49.3848079176936,76.0204693936602)) ;
#9166 = CARTESIAN_POINT('Ctrl Pts',(23.5203694574972,49.3747203101764,76.0204384892973)) ;
#9167 = CARTESIAN_POINT('Ctrl Pts',(23.5264510044697,49.364632925956,76.0204004728069)) ;
#9168 = CARTESIAN_POINT('Ctrl Pts',(23.681442216326,49.1075509841643,76.0194316038757)) ;
#9169 = CARTESIAN_POINT('Ctrl Pts',(23.8365783763701,48.8504690628024,76.0138346276243)) ;
#9170 = CARTESIAN_POINT('Ctrl Pts',(23.9913881239066,48.5931578990174,76.0036143155886)) ;
#9171 = CARTESIAN_POINT('Ctrl Pts',(23.9994194115387,48.5798089981878,76.0030841017813)) ;
#9172 = CARTESIAN_POINT('Ctrl Pts',(24.0074500682842,48.566459068981,76.0025414286173)) ;
#9173 = CARTESIAN_POINT('Ctrl Pts',(24.0154800122403,48.5531081058639,76.0019862962604)) ;
#9174 = CARTESIAN_POINT('Ctrl Pts',(24.1683073257374,48.2990102146546,75.9914209190658)) ;
#9175 = CARTESIAN_POINT('Ctrl Pts',(24.320977601014,48.0446012919295,75.9763394192743)) ;
#9176 = CARTESIAN_POINT('Ctrl Pts',(24.4731100447151,47.7903648312084,75.9567599665068)) ;
#9177 = CARTESIAN_POINT('Ctrl Pts',(24.4830339125752,47.7737805380753,75.9554827642394)) ;
#9178 = CARTESIAN_POINT('Ctrl Pts',(24.492955861141,47.7571963611373,75.9541863741319)) ;
#9179 = CARTESIAN_POINT('Ctrl Pts',(24.50287583425,47.7406123516807,75.9528707946832)) ;
#9180 = CARTESIAN_POINT('Ctrl Pts',(24.6530188950513,47.4896062337405,75.9329589337344)) ;
#9181 = CARTESIAN_POINT('Ctrl Pts',(24.8023159560001,47.2387261489803,75.9087129990594)) ;
#9182 = CARTESIAN_POINT('Ctrl Pts',(24.9508196300929,46.9878897404751,75.8801450477756)) ;
#9183 = CARTESIAN_POINT('Ctrl Pts',(24.9625073132173,46.9681481652139,75.8778966646015)) ;
#9184 = CARTESIAN_POINT('Ctrl Pts',(24.9741897307449,46.9484074501543,75.8756215645657)) ;
#9185 = CARTESIAN_POINT('Ctrl Pts',(24.9858668886883,46.9286675886392,75.8733197584537)) ;
#9186 = CARTESIAN_POINT('Ctrl Pts',(25.1323624947587,46.6810214584402,75.8444424851415)) ;
#9187 = CARTESIAN_POINT('Ctrl Pts',(25.2781273118314,46.4334531760666,75.8113320199874)) ;
#9188 = CARTESIAN_POINT('Ctrl Pts',(25.4227590725841,46.1857600468476,75.7740795212884)) ;
#9189 = CARTESIAN_POINT('Ctrl Pts',(25.4360537096591,46.1629919477676,75.7706552495533)) ;
#9190 = CARTESIAN_POINT('Ctrl Pts',(25.4493390556513,46.140222308408,75.7671959063944)) ;
#9191 = CARTESIAN_POINT('Ctrl Pts',(25.4626147718347,46.1174510138861,75.7637015657915)) ;
#9192 = CARTESIAN_POINT('Ctrl Pts',(25.6052771603323,45.8727480373531,75.7261509756951)) ;
#9193 = CARTESIAN_POINT('Ctrl Pts',(25.7469101647593,45.6279743432129,75.6845467079578)) ;
#9194 = CARTESIAN_POINT('Ctrl Pts',(25.8874434877188,45.3830610445957,75.638885508351)) ;
#9195 = CARTESIAN_POINT('',(25.8068141710837,48.5844537758935,103.144850199241)) ;
#9196 = CARTESIAN_POINT('Ctrl Pts',(32.2277008466604,45.3830585486371,95.1522036362991)) ;
#9197 = CARTESIAN_POINT('Ctrl Pts',(32.3031100938315,45.4231928249935,95.6688829820357)) ;
#9198 = CARTESIAN_POINT('Ctrl Pts',(32.320119173168,45.4870033446877,96.190162540208)) ;
#9199 = CARTESIAN_POINT('Ctrl Pts',(32.2390995479676,45.6539797372435,97.2319881208699)) ;
#9200 = CARTESIAN_POINT('Ctrl Pts',(32.1390467146082,45.7573388893141,97.7487283877929)) ;
#9201 = CARTESIAN_POINT('Ctrl Pts',(31.7108073456657,46.0833507061677,99.1224310140683)) ;
#9202 = CARTESIAN_POINT('Ctrl Pts',(31.2706997360599,46.3336877227689,99.9279524714847)) ;
#9203 = CARTESIAN_POINT('Ctrl Pts',(30.0747052050763,46.9107591797133,101.375467312635)) ;
#9204 = CARTESIAN_POINT('Ctrl Pts',(29.3055362183394,47.2383195349502,101.98507439633)) ;
#9205 = CARTESIAN_POINT('Ctrl Pts',(27.6191245040703,47.9083523080808,102.832323345458)) ;
#9206 = CARTESIAN_POINT('Ctrl Pts',(26.722903131973,48.2450338483641,103.078492136777)) ;
#9207 = CARTESIAN_POINT('Ctrl Pts',(25.8068141710837,48.5844537758935,103.144850199241)) ;
#9208 = CARTESIAN_POINT('',(25.7569277250234,48.6029307720944,103.148213134921)) ;
#9209 = CARTESIAN_POINT('Origin',(28.1803190987662,48.3559725194583,140.311274111017)) ;
#9210 = CARTESIAN_POINT('',(8.73526681379954,55.0677871747466,99.9661893007231)) ;
#9211 = CARTESIAN_POINT('Ctrl Pts',(25.7569277250234,48.6029307720944,103.148213134921)) ;
#9212 = CARTESIAN_POINT('Ctrl Pts',(25.2643121406148,48.785356686239,103.180289412696)) ;
#9213 = CARTESIAN_POINT('Ctrl Pts',(24.7709904943805,48.9676174488035,103.198530845007)) ;
#9214 = CARTESIAN_POINT('Ctrl Pts',(23.1539479349856,49.5650439193917,103.258323827163)) ;
#9215 = CARTESIAN_POINT('Ctrl Pts',(21.5382863937015,50.16247038998,103.168659878861)) ;
#9216 = CARTESIAN_POINT('Ctrl Pts',(19.9226248524173,50.7598968605682,103.078995930559)) ;
#9217 = CARTESIAN_POINT('Ctrl Pts',(18.3221285838481,51.3573233311564,102.840640032991)) ;
#9218 = CARTESIAN_POINT('Ctrl Pts',(16.7216323152788,51.9547498017447,102.602284135423)) ;
#9219 = CARTESIAN_POINT('Ctrl Pts',(15.1499561892687,52.5521762723329,102.217269857065)) ;
#9220 = CARTESIAN_POINT('Ctrl Pts',(13.5782800632586,53.1496027429211,101.832255578707)) ;
#9221 = CARTESIAN_POINT('Ctrl Pts',(12.0488330663575,53.7470292135094,101.30386772563)) ;
#9222 = CARTESIAN_POINT('Ctrl Pts',(10.5193860694563,54.3444556840976,100.775479872552)) ;
#9223 = CARTESIAN_POINT('Ctrl Pts',(9.04521690417374,54.9418821546858,100.108226463614)) ;
#9224 = CARTESIAN_POINT('Ctrl Pts',(8.88991083437399,55.0048219850164,100.0379302541)) ;
#9225 = CARTESIAN_POINT('Ctrl Pts',(8.73526681379953,55.0677871747466,99.9661893007231)) ;
#9226 = CARTESIAN_POINT('',(8.68996421845689,55.0862551252693,99.9450317561577)) ;
#9227 = CARTESIAN_POINT('Origin',(-6.32810000537899,55.5493242894856,132.402663943764)) ;
#9228 = CARTESIAN_POINT('Ctrl Pts',(8.68996421845687,55.0862551252692,99.9450317561577)) ;
#9229 = CARTESIAN_POINT('Ctrl Pts',(8.20077668425168,55.2861476427454,99.7135814400466)) ;
#9230 = CARTESIAN_POINT('Ctrl Pts',(7.73969544475074,55.4856144064204,99.4260005287769)) ;
#9231 = CARTESIAN_POINT('Ctrl Pts',(6.86222930708719,55.8948727823203,98.7254146660119)) ;
#9232 = CARTESIAN_POINT('Ctrl Pts',(6.45404498576417,56.1030297966035,98.3070128505722)) ;
#9233 = CARTESIAN_POINT('Ctrl Pts',(5.52344278067351,56.6395229540351,97.0772238444848)) ;
#9234 = CARTESIAN_POINT('Ctrl Pts',(5.1037113359308,56.9553077214542,96.1962925358796)) ;
#9235 = CARTESIAN_POINT('Ctrl Pts',(4.66774586592465,57.5027528833965,94.3787099674685)) ;
#9236 = CARTESIAN_POINT('Ctrl Pts',(4.62591980549989,57.7356392971192,93.4655076450606)) ;
#9237 = CARTESIAN_POINT('Ctrl Pts',(4.86507457348184,58.0583687617078,91.8978184860504)) ;
#9238 = CARTESIAN_POINT('Ctrl Pts',(5.06231793135134,58.1679507457142,91.2466136289794)) ;
#9239 = CARTESIAN_POINT('Ctrl Pts',(5.60181878346812,58.3023924932056,90.1031845606475)) ;
#9240 = CARTESIAN_POINT('Ctrl Pts',(5.91644124082818,58.3364158757984,89.6072507467857)) ;
#9241 = CARTESIAN_POINT('Ctrl Pts',(6.29012224935736,58.3353824278239,89.1555480018396)) ;
#9242 = CARTESIAN_POINT('Ctrl Pts',(34.3883885914319,45.3830585852922,101.478510132603)) ;
#9243 = CARTESIAN_POINT('Ctrl Pts',(32.8508673372113,45.9804850758286,101.982942280144)) ;
#9244 = CARTESIAN_POINT('Ctrl Pts',(31.2733617497745,46.5779115664505,102.343358040426)) ;
#9245 = CARTESIAN_POINT('Ctrl Pts',(29.6958562152367,47.1753380370388,102.703773788621)) ;
#9246 = CARTESIAN_POINT('Ctrl Pts',(28.0918250713921,47.772764507627,102.917098219058)) ;
#9247 = CARTESIAN_POINT('Ctrl Pts',(26.4877939275474,48.3701909782152,103.130422649496)) ;
#9248 = CARTESIAN_POINT('Ctrl Pts',(24.8709222025499,48.9676174488035,103.19483575335)) ;
#9249 = CARTESIAN_POINT('Ctrl Pts',(23.2540504775523,49.5650439193917,103.259248857204)) ;
#9250 = CARTESIAN_POINT('Ctrl Pts',(21.6381327508665,50.16247038998,103.174201084585)) ;
#9251 = CARTESIAN_POINT('Ctrl Pts',(20.0222150241807,50.7598968605682,103.089153311966)) ;
#9252 = CARTESIAN_POINT('Ctrl Pts',(18.4210377360943,51.3573233311564,102.855370260482)) ;
#9253 = CARTESIAN_POINT('Ctrl Pts',(16.8198604480078,51.9547498017447,102.621587208999)) ;
#9254 = CARTESIAN_POINT('Ctrl Pts',(15.2470842785835,52.5521762723329,102.241063433216)) ;
#9255 = CARTESIAN_POINT('Ctrl Pts',(13.6743081091592,53.1496027429211,101.860539657434)) ;
#9256 = CARTESIAN_POINT('Ctrl Pts',(12.1433514301292,53.7470292135094,101.336521652039)) ;
#9257 = CARTESIAN_POINT('Ctrl Pts',(10.6123947510992,54.3444556840976,100.812503646644)) ;
#9258 = CARTESIAN_POINT('Ctrl Pts',(9.13631914504893,54.9418821546858,100.149462148494)) ;
#9259 = CARTESIAN_POINT('Ctrl Pts',(7.66024353899866,55.5393086252741,99.4864206503448)) ;
#9260 = CARTESIAN_POINT('Ctrl Pts',(6.25164236254934,56.1367350958623,98.6900124957215)) ;
#9261 = CARTESIAN_POINT('Ctrl Pts',(4.84304118610003,56.7341615664505,97.8936043410982)) ;
#9262 = CARTESIAN_POINT('Ctrl Pts',(3.51393212783033,57.3315880370388,96.9706242035708)) ;
#9263 = CARTESIAN_POINT('Ctrl Pts',(2.34451316548462,57.857234776835,96.1585384924868)) ;
#9264 = CARTESIAN_POINT('Ctrl Pts',(1.24491679165593,58.3831186720347,95.2541537699803)) ;
#9265 = CARTESIAN_POINT('Ctrl Pts',(25.8904211471758,45.3830585852922,75.3244559053118)) ;
#9266 = CARTESIAN_POINT('Ctrl Pts',(25.5620748354161,45.9804850758286,75.4360032937205)) ;
#9267 = CARTESIAN_POINT('Ctrl Pts',(25.2248368963556,46.5779115664506,75.5167788640701)) ;
#9268 = CARTESIAN_POINT('Ctrl Pts',(24.8875989686039,47.1753380370388,75.5975544317111)) ;
#9269 = CARTESIAN_POINT('Ctrl Pts',(24.5443466092877,47.772764507627,75.6468690346784)) ;
#9270 = CARTESIAN_POINT('Ctrl Pts',(24.2010942499714,48.3701909782152,75.6961836376457)) ;
#9271 = CARTESIAN_POINT('Ctrl Pts',(23.854755967193,48.9676174488035,75.7136165411346)) ;
#9272 = CARTESIAN_POINT('Ctrl Pts',(23.5084176844145,49.5650439193917,75.7310494446235)) ;
#9273 = CARTESIAN_POINT('Ctrl Pts',(23.1619483142871,50.16247038998,75.7164519172482)) ;
#9274 = CARTESIAN_POINT('Ctrl Pts',(22.8154789441596,50.7598968605682,75.7018543898729)) ;
#9275 = CARTESIAN_POINT('Ctrl Pts',(22.4718344411874,51.3573233311564,75.6553509725899)) ;
#9276 = CARTESIAN_POINT('Ctrl Pts',(22.1281899382152,51.9547498017447,75.608847555307)) ;
#9277 = CARTESIAN_POINT('Ctrl Pts',(21.7903021561321,52.5521762723329,75.530834998876)) ;
#9278 = CARTESIAN_POINT('Ctrl Pts',(21.4524143740489,53.1496027429211,75.452822442445)) ;
#9279 = CARTESIAN_POINT('Ctrl Pts',(21.1231660522755,53.7470292135094,75.3439663224911)) ;
#9280 = CARTESIAN_POINT('Ctrl Pts',(20.7939177305022,54.3444556840976,75.2351102025371)) ;
#9281 = CARTESIAN_POINT('Ctrl Pts',(20.4761178996304,54.9418821546858,75.096339241094)) ;
#9282 = CARTESIAN_POINT('Ctrl Pts',(20.1583180687586,55.5393086252741,74.9575682796509)) ;
#9283 = CARTESIAN_POINT('Ctrl Pts',(19.8546780848923,56.1367350958623,74.7900664216324)) ;
#9284 = CARTESIAN_POINT('Ctrl Pts',(19.551038101026,56.7341615664506,74.6225645636139)) ;
#9285 = CARTESIAN_POINT('Ctrl Pts',(19.264148513447,57.3315880370388,74.4277608758131)) ;
#9286 = CARTESIAN_POINT('Ctrl Pts',(19.0117282009625,57.8572347768351,74.2563625055804)) ;
#9287 = CARTESIAN_POINT('Ctrl Pts',(18.7740631193741,58.3831186720347,74.0650284404828)) ;
#9288 = CARTESIAN_POINT('',(18.5858460045131,58.3830537363182,74.292544600312)) ;
#9289 = CARTESIAN_POINT('Ctrl Pts',(25.9816821278123,45.3830674541116,75.6052810522977)) ;
#9290 = CARTESIAN_POINT('Ctrl Pts',(25.9720536409296,45.3999249614356,75.6085466570867)) ;
#9291 = CARTESIAN_POINT('Ctrl Pts',(25.9622835986064,45.4170195560991,75.6118389611852)) ;
#9292 = CARTESIAN_POINT('Ctrl Pts',(25.9428699827234,45.450966082336,75.6183380969714)) ;
#9293 = CARTESIAN_POINT('Ctrl Pts',(25.9331581705972,45.4679374856696,75.6215680725326)) ;
#9294 = CARTESIAN_POINT('Ctrl Pts',(25.9040078813387,45.5188462146271,75.6311992306336)) ;
#9295 = CARTESIAN_POINT('Ctrl Pts',(25.8845545514463,45.5527780591992,75.6375416449359)) ;
#9296 = CARTESIAN_POINT('Ctrl Pts',(25.8261364256564,45.6545524513434,75.6563338676956)) ;
#9297 = CARTESIAN_POINT('Ctrl Pts',(25.7871134891735,45.7223738576059,75.6685486410987)) ;
#9298 = CARTESIAN_POINT('Ctrl Pts',(25.6987804559921,45.8755455989773,75.6954380806355)) ;
#9299 = CARTESIAN_POINT('Ctrl Pts',(25.6494252923191,45.9608834226817,75.709929590608)) ;
#9300 = CARTESIAN_POINT('Ctrl Pts',(25.5708698027494,46.096346675625,75.7321540649685)) ;
#9301 = CARTESIAN_POINT('Ctrl Pts',(25.5417333879409,46.1464973799218,75.7402142926808)) ;
#9302 = CARTESIAN_POINT('Ctrl Pts',(25.3777882376432,46.4282028809694,75.7845431297761)) ;
#9303 = CARTESIAN_POINT('Ctrl Pts',(25.2421515380204,46.6594344485447,75.8173327836383)) ;
#9304 = CARTESIAN_POINT('Ctrl Pts',(25.082837649862,46.9296827699039,75.8513551760635)) ;
#9305 = CARTESIAN_POINT('Ctrl Pts',(25.0597605868494,46.968795042417,75.8561741409081)) ;
#9306 = CARTESIAN_POINT('Ctrl Pts',(24.8937141271844,47.2499758749388,75.8900633827158)) ;
#9307 = CARTESIAN_POINT('Ctrl Pts',(24.7501105114405,47.4918541916406,75.9151945113985)) ;
#9308 = CARTESIAN_POINT('Ctrl Pts',(24.4382706209287,48.0143150858147,75.9608047711095)) ;
#9309 = CARTESIAN_POINT('Ctrl Pts',(24.2699414562195,48.2952954282308,75.9798403599875)) ;
#9310 = CARTESIAN_POINT('Ctrl Pts',(24.0910078683281,48.5931204307079,75.9941989442598)) ;
#9311 = CARTESIAN_POINT('Ctrl Pts',(24.0807918914205,48.6101204742723,75.9949984353586)) ;
#9312 = CARTESIAN_POINT('Ctrl Pts',(23.9119431175511,48.8910362150329,76.0078771021127)) ;
#9313 = CARTESIAN_POINT('Ctrl Pts',(23.7528087469497,49.1549226796789,76.0151262737856)) ;
#9314 = CARTESIAN_POINT('Ctrl Pts',(23.5900902749489,49.4249376060057,76.0175458523535)) ;
#9315 = CARTESIAN_POINT('Ctrl Pts',(23.5865567043535,49.430801123754,76.0175959960367)) ;
#9316 = CARTESIAN_POINT('Ctrl Pts',(23.420298917879,49.7066812295575,76.0198423852037)) ;
#9317 = CARTESIAN_POINT('Ctrl Pts',(23.2573680914076,49.9768666464288,76.0169512266826)) ;
#9318 = CARTESIAN_POINT('Ctrl Pts',(23.0912143366874,50.2527043291671,76.0087719319334)) ;
#9319 = CARTESIAN_POINT('Ctrl Pts',(23.0879880363181,50.2580605419638,76.0086111000024)) ;
#9320 = CARTESIAN_POINT('Ctrl Pts',(22.9250557359098,50.5285623062303,76.0003873586263)) ;
#9321 = CARTESIAN_POINT('Ctrl Pts',(22.7655562097403,50.794089282034,75.9874165770804)) ;
#9322 = CARTESIAN_POINT('Ctrl Pts',(22.596220584203,51.0767673302901,75.9683691764023)) ;
#9323 = CARTESIAN_POINT('Ctrl Pts',(22.5861929542279,51.09350971285,75.9672215336923)) ;
#9324 = CARTESIAN_POINT('Ctrl Pts',(22.4915033167505,51.2516332986598,75.9561983324922)) ;
#9325 = CARTESIAN_POINT('Ctrl Pts',(22.4068327694471,51.3931664826184,75.944930972281)) ;
#9326 = CARTESIAN_POINT('Ctrl Pts',(22.2548906854115,51.6479675595709,75.922163245892)) ;
#9327 = CARTESIAN_POINT('Ctrl Pts',(22.1875111509901,51.7612319406822,75.9111590655696)) ;
#9328 = CARTESIAN_POINT('Ctrl Pts',(22.1035923597581,51.9026374456282,75.8963208743334)) ;
#9329 = CARTESIAN_POINT('Ctrl Pts',(22.0868835458075,51.9308091085122,75.8933101583207)) ;
#9330 = CARTESIAN_POINT('Ctrl Pts',(21.9025872293205,52.2417252333167,75.8594806951164)) ;
#9331 = CARTESIAN_POINT('Ctrl Pts',(21.7360368649525,52.5241195492734,75.8232276595509)) ;
#9332 = CARTESIAN_POINT('Ctrl Pts',(21.4355297941431,53.0381974993209,75.7474217195157)) ;
#9333 = CARTESIAN_POINT('Ctrl Pts',(21.3011963380331,53.2697333986845,75.7096734001977)) ;
#9334 = CARTESIAN_POINT('Ctrl Pts',(21.1385342177892,53.5522259966922,75.6592141409401)) ;
#9335 = CARTESIAN_POINT('Ctrl Pts',(21.109245102224,53.6031771340245,75.6499383146778)) ;
#9336 = CARTESIAN_POINT('Ctrl Pts',(20.9536831119847,53.8742457620906,75.599659155911)) ;
#9337 = CARTESIAN_POINT('Ctrl Pts',(20.8283529470414,54.0945463050606,75.5555823028404)) ;
#9338 = CARTESIAN_POINT('Ctrl Pts',(20.6690101501099,54.3774106831927,75.4949256517854)) ;
#9339 = CARTESIAN_POINT('Ctrl Pts',(20.6339184787535,54.4398806254215,75.48127574604)) ;
#9340 = CARTESIAN_POINT('Ctrl Pts',(20.481821152551,54.711432139282,75.4208404961403)) ;
#9341 = CARTESIAN_POINT('Ctrl Pts',(20.3657022613531,54.9205828276725,75.3714026715031)) ;
#9342 = CARTESIAN_POINT('Ctrl Pts',(20.2104748018518,55.203368432954,75.3008285804407)) ;
#9343 = CARTESIAN_POINT('Ctrl Pts',(20.1700922605189,55.2772338818091,75.2820492977946)) ;
#9344 = CARTESIAN_POINT('Ctrl Pts',(20.0224335966246,55.5485088102294,75.2118349432992)) ;
#9345 = CARTESIAN_POINT('Ctrl Pts',(19.916228046497,55.7457837763575,75.1583211431054)) ;
#9346 = CARTESIAN_POINT('Ctrl Pts',(19.7659277041273,56.0282588904728,75.0782259130373)) ;
#9347 = CARTESIAN_POINT('Ctrl Pts',(19.720810206197,56.1134884206069,75.0536060353448)) ;
#9348 = CARTESIAN_POINT('Ctrl Pts',(19.5781288974087,56.3844426291216,74.9739057491897)) ;
#9349 = CARTESIAN_POINT('Ctrl Pts',(19.481611211323,56.5701302611202,74.9172297832555)) ;
#9350 = CARTESIAN_POINT('Ctrl Pts',(19.3366723231393,56.8526653482991,74.8278700217508)) ;
#9351 = CARTESIAN_POINT('Ctrl Pts',(19.2873541178717,56.9494716030763,74.7966940866653)) ;
#9352 = CARTESIAN_POINT('Ctrl Pts',(19.1502669264902,57.2204413601227,74.7078682177841)) ;
#9353 = CARTESIAN_POINT('Ctrl Pts',(19.0632399891367,57.394657675533,74.6489470349753)) ;
#9354 = CARTESIAN_POINT('Ctrl Pts',(18.9240097385661,57.6774250653638,74.5505202852794)) ;
#9355 = CARTESIAN_POINT('Ctrl Pts',(18.8710615649226,57.7859396412685,74.5120812548434)) ;
#9356 = CARTESIAN_POINT('Ctrl Pts',(18.8055003584704,57.9216227418848,74.4632125950281)) ;
#9357 = CARTESIAN_POINT('Ctrl Pts',(18.7924327198245,57.948727891259,74.4534079705152)) ;
#9358 = CARTESIAN_POINT('Ctrl Pts',(18.7467598748858,58.0436810159814,74.4189146837387)) ;
#9359 = CARTESIAN_POINT('Ctrl Pts',(18.7143072863786,58.1115399743058,74.394001847081)) ;
#9360 = CARTESIAN_POINT('Ctrl Pts',(18.6659139020866,58.2133484522828,74.356242806694)) ;
#9361 = CARTESIAN_POINT('Ctrl Pts',(18.6498317153866,58.2472850649065,74.3435925846863)) ;
#9362 = CARTESIAN_POINT('Ctrl Pts',(18.6257803686513,58.2981973836588,74.3245201977021)) ;
#9363 = CARTESIAN_POINT('Ctrl Pts',(18.6177752421485,58.3151693899113,74.3181465595116)) ;
#9364 = CARTESIAN_POINT('Ctrl Pts',(18.607604619674,58.3367668565651,74.3100160221478)) ;
#9365 = CARTESIAN_POINT('Ctrl Pts',(18.6054237775714,58.3413999128696,74.3082707117144)) ;
#9366 = CARTESIAN_POINT('Ctrl Pts',(18.5974199895112,58.3584108602029,74.3018582790177)) ;
#9367 = CARTESIAN_POINT('Ctrl Pts',(18.5915987969254,58.3707975233387,74.2971806666215)) ;
#9368 = CARTESIAN_POINT('Ctrl Pts',(18.5858469328057,58.3830508753329,74.2925453446431)) ;
#9369 = CARTESIAN_POINT('',(6.29012224935737,58.3831162793798,89.1555480018396)) ;
#9370 = CARTESIAN_POINT('Ctrl Pts',(18.5858590582705,58.3830900980199,74.2925553933006)) ;
#9371 = CARTESIAN_POINT('Ctrl Pts',(16.5365695895273,58.383105259385,76.7697208287716)) ;
#9372 = CARTESIAN_POINT('Ctrl Pts',(14.4872801207512,58.3831073991803,79.2468862642824)) ;
#9373 = CARTESIAN_POINT('Ctrl Pts',(10.3887011844437,58.3831134572106,84.2012171337991)) ;
#9374 = CARTESIAN_POINT('Ctrl Pts',(8.33941171690048,58.3831150235129,86.6783825678194)) ;
#9375 = CARTESIAN_POINT('Ctrl Pts',(6.2901222493574,58.3831162793798,89.1555480018396)) ;
#9376 = CARTESIAN_POINT('',(8.73523672734845,55.104724217109,99.9662540836333)) ;
#9377 = CARTESIAN_POINT('Ctrl Pts',(6.29012224935736,58.3831162793798,89.1555480018396)) ;
#9378 = CARTESIAN_POINT('Ctrl Pts',(5.91420081213285,58.3831165097559,89.6099589598563)) ;
#9379 = CARTESIAN_POINT('Ctrl Pts',(5.59809067175723,58.3477204548742,90.1090822491473)) ;
#9380 = CARTESIAN_POINT('Ctrl Pts',(5.05681898264549,58.2097833704153,91.2606504993859)) ;
#9381 = CARTESIAN_POINT('Ctrl Pts',(4.85984853002451,58.0979491851445,91.9168709057473)) ;
#9382 = CARTESIAN_POINT('Ctrl Pts',(4.62536151099518,57.7707078254696,93.4903816655359)) ;
#9383 = CARTESIAN_POINT('Ctrl Pts',(4.67047634429036,57.5360202457534,94.4039684820573)) ;
#9384 = CARTESIAN_POINT('Ctrl Pts',(5.11328015675259,56.9856758817168,96.220706550885)) ;
#9385 = CARTESIAN_POINT('Ctrl Pts',(5.53647004679195,56.6687344805943,97.1004478735331)) ;
#9386 = CARTESIAN_POINT('Ctrl Pts',(6.47458953048251,56.1294192803767,98.3303404896527)) ;
#9387 = CARTESIAN_POINT('Ctrl Pts',(6.88771640637359,55.9194276565173,98.7498321799113)) ;
#9388 = CARTESIAN_POINT('Ctrl Pts',(7.77518736240662,55.5068628236254,99.4502708040986)) ;
#9389 = CARTESIAN_POINT('Ctrl Pts',(8.24115253357343,55.3059550653477,99.7367917164622)) ;
#9390 = CARTESIAN_POINT('Ctrl Pts',(8.73523672734845,55.104724217109,99.9662540836333)) ;
#9391 = CARTESIAN_POINT('',(25.7569323765141,48.6398835186857,103.148284411731)) ;
#9392 = CARTESIAN_POINT('Ctrl Pts',(25.7569323765141,48.6398835186857,103.148284411731)) ;
#9393 = CARTESIAN_POINT('Ctrl Pts',(25.3142223238036,48.8038201453524,103.177175458668)) ;
#9394 = CARTESIAN_POINT('Ctrl Pts',(24.8709222003948,48.9676174488035,103.194835695068)) ;
#9395 = CARTESIAN_POINT('Ctrl Pts',(23.2540504780917,49.5650439193917,103.259248798822)) ;
#9396 = CARTESIAN_POINT('Ctrl Pts',(21.6381327540982,50.16247038998,103.174201026353)) ;
#9397 = CARTESIAN_POINT('Ctrl Pts',(20.0222150301047,50.7598968605682,103.089153253883)) ;
#9398 = CARTESIAN_POINT('Ctrl Pts',(18.4210377446852,51.3573233311564,102.855370202796)) ;
#9399 = CARTESIAN_POINT('Ctrl Pts',(16.8198604592657,51.9547498017447,102.62158715171)) ;
#9400 = CARTESIAN_POINT('Ctrl Pts',(15.2470842924603,52.5521762723329,102.241063376569)) ;
#9401 = CARTESIAN_POINT('Ctrl Pts',(13.6743081256549,53.1496027429211,101.860539601428)) ;
#9402 = CARTESIAN_POINT('Ctrl Pts',(12.1433514491735,53.7470292135094,101.336521596914)) ;
#9403 = CARTESIAN_POINT('Ctrl Pts',(10.6123947726921,54.3444556840976,100.812503592399)) ;
#9404 = CARTESIAN_POINT('Ctrl Pts',(9.13631916909835,54.9418821546858,100.149462095362)) ;
#9405 = CARTESIAN_POINT('Ctrl Pts',(8.93520090615318,55.0232827101246,100.059121360903)) ;
#9406 = CARTESIAN_POINT('Ctrl Pts',(8.73523672734845,55.104724217109,99.9662540836333)) ;
#9407 = CARTESIAN_POINT('Ctrl Pts',(25.7569323765141,48.6398835186857,103.148284411731)) ;
#9408 = CARTESIAN_POINT('Ctrl Pts',(26.2971586435828,48.4398363968329,103.113029503144)) ;
#9409 = CARTESIAN_POINT('Ctrl Pts',(26.8319085774414,48.2402511072952,103.015193960956)) ;
#9410 = CARTESIAN_POINT('Ctrl Pts',(27.9052437457281,47.8311034847338,102.686568200856)) ;
#9411 = CARTESIAN_POINT('Ctrl Pts',(28.4381823878521,47.6231197022397,102.447937978474)) ;
#9412 = CARTESIAN_POINT('Ctrl Pts',(29.755590053916,47.0862681322598,101.647310522153)) ;
#9413 = CARTESIAN_POINT('Ctrl Pts',(30.4702215873772,46.7703270771007,100.982603468591)) ;
#9414 = CARTESIAN_POINT('Ctrl Pts',(31.545074951219,46.2216257312612,99.4520955884149)) ;
#9415 = CARTESIAN_POINT('Ctrl Pts',(31.920053706703,45.9879058539332,98.6179275795044)) ;
#9416 = CARTESIAN_POINT('Ctrl Pts',(32.2740982535239,45.6640068779433,97.0725188928857)) ;
#9417 = CARTESIAN_POINT('Ctrl Pts',(32.3302213337266,45.5539383973837,96.3954399628129)) ;
#9418 = CARTESIAN_POINT('Ctrl Pts',(32.2496293109684,45.4179657782124,95.134669592589)) ;
#9419 = CARTESIAN_POINT('Ctrl Pts',(32.1396710614035,45.3830586252741,94.557669561118)) ;
#9420 = CARTESIAN_POINT('Ctrl Pts',(31.9584809790255,45.3830586252741,94.000023827484)) ;
#9421 = CARTESIAN_POINT('Origin',(25.3010853649595,45.3822493559848,96.1631427881087)) ;
#9422 = CARTESIAN_POINT('',(25.7569323765141,45.3822493559848,103.148284411731)) ;
#9423 = CARTESIAN_POINT('Origin',(23.47768801576,45.3822493559848,68.2224337400009)) ;
#9424 = CARTESIAN_POINT('',(8.73523672734845,45.3822493559848,99.9662540836333)) ;
#9425 = CARTESIAN_POINT('Origin',(11.6837149504503,45.3822493559848,93.6175159280709)) ;
#9426 = CARTESIAN_POINT('',(6.29012224935737,45.3822493559848,89.1555480018396)) ;
#9427 = CARTESIAN_POINT('Origin',(18.7740766870781,45.3822493559848,74.0650393632132)) ;
#9428 = CARTESIAN_POINT('Ctrl Pts',(18.7107542394381,57.826549970365,74.1415830535878)) ;
#9429 = CARTESIAN_POINT('Ctrl Pts',(18.7107226067175,57.8721147557093,74.1416212909784)) ;
#9430 = CARTESIAN_POINT('Ctrl Pts',(18.708092508703,57.9184467892871,74.1448005333832)) ;
#9431 = CARTESIAN_POINT('Ctrl Pts',(18.6973298341945,58.006695871061,74.1578103720089)) ;
#9432 = CARTESIAN_POINT('Ctrl Pts',(18.6890653833466,58.0508719526447,74.1678003769401)) ;
#9433 = CARTESIAN_POINT('Ctrl Pts',(18.66602343776,58.1278680024908,74.1956533045249)) ;
#9434 = CARTESIAN_POINT('Ctrl Pts',(18.6527112796475,58.1579990081032,74.2117449394387)) ;
#9435 = CARTESIAN_POINT('Ctrl Pts',(18.6298766097115,58.1911673829066,74.2393473138024)) ;
#9436 = CARTESIAN_POINT('Ctrl Pts',(18.6208888935898,58.2011153712953,74.2502115962984)) ;
#9437 = CARTESIAN_POINT('Ctrl Pts',(18.6025171726295,58.2136587167219,74.272419192076)) ;
#9438 = CARTESIAN_POINT('Ctrl Pts',(18.593643669708,58.2169692427703,74.2831454145369)) ;
#9439 = CARTESIAN_POINT('Ctrl Pts',(18.5844571388615,58.2172758076351,74.2942500227594)) ;
#9440 = CARTESIAN_POINT('Ctrl Pts',(18.5858591957557,58.3830247512599,74.2925552271096)) ;
#9441 = CARTESIAN_POINT('Ctrl Pts',(18.5903405925418,58.3830247228371,74.2871381489514)) ;
#9442 = CARTESIAN_POINT('Ctrl Pts',(18.5947855070738,58.3837424765035,74.2817651702627)) ;
#9443 = CARTESIAN_POINT('Ctrl Pts',(18.6038618438227,58.3866521090648,74.2707937638226)) ;
#9444 = CARTESIAN_POINT('Ctrl Pts',(18.6084152748266,58.3889169428568,74.2652896112528)) ;
#9445 = CARTESIAN_POINT('Ctrl Pts',(18.6229204567539,58.3985444430684,74.2477558582845)) ;
#9446 = CARTESIAN_POINT('Ctrl Pts',(18.6320253163883,58.4085611720381,74.2367499735612)) ;
#9447 = CARTESIAN_POINT('Ctrl Pts',(18.6544021729805,58.4411881110096,74.2097010004657)) ;
#9448 = CARTESIAN_POINT('Ctrl Pts',(18.6672182435102,58.4701790972226,74.1942090324728)) ;
#9449 = CARTESIAN_POINT('Ctrl Pts',(18.6896541908679,58.5450324120245,74.167088630912)) ;
#9450 = CARTESIAN_POINT('Ctrl Pts',(18.6977191225924,58.5884045334883,74.1573398030111)) ;
#9451 = CARTESIAN_POINT('Ctrl Pts',(18.7082226594837,58.6752752681701,74.144643207955)) ;
#9452 = CARTESIAN_POINT('Ctrl Pts',(18.710754102308,58.721038685503,74.1415832193495)) ;
#9453 = CARTESIAN_POINT('Ctrl Pts',(18.7107539231051,58.7660385537516,74.1415834359687)) ;
#9454 = CARTESIAN_POINT('Ctrl Pts',(18.5483450846703,58.2943663992286,74.2649701337207)) ;
#9455 = CARTESIAN_POINT('Ctrl Pts',(18.6732965800537,58.2924602039142,74.1136194276355)) ;
#9456 = CARTESIAN_POINT('Ctrl Pts',(18.5454318956407,58.191081348463,74.0045483675006)) ;
#9457 = CARTESIAN_POINT('Ctrl Pts',(18.8016527608616,57.752299968185,74.4716103680308)) ;
#9458 = CARTESIAN_POINT('Ctrl Pts',(18.9202592219973,57.7503889244304,74.31502434924)) ;
#9459 = CARTESIAN_POINT('Ctrl Pts',(18.7878340776408,57.6489874075623,74.2113221384691)) ;
#9460 = CARTESIAN_POINT('Ctrl Pts',(19.0675721711253,57.2111033102809,74.6619872725778)) ;
#9461 = CARTESIAN_POINT('Ctrl Pts',(19.1795133398185,57.2091968025493,74.5005686455089)) ;
#9462 = CARTESIAN_POINT('Ctrl Pts',(19.0428275223573,57.1078632090634,74.4024821086413)) ;
#9463 = CARTESIAN_POINT('Ctrl Pts',(19.4822900636562,56.3997926693349,74.9212423510824)) ;
#9464 = CARTESIAN_POINT('Ctrl Pts',(19.5838324114684,56.3978864499649,74.7532373532317)) ;
#9465 = CARTESIAN_POINT('Ctrl Pts',(19.4413748489443,56.2965290900091,74.6639725606601)) ;
#9466 = CARTESIAN_POINT('Ctrl Pts',(19.6233067304825,56.1295297083821,75.0033649035992)) ;
#9467 = CARTESIAN_POINT('Ctrl Pts',(19.7213132030636,56.1276240321501,74.8332713211198)) ;
#9468 = CARTESIAN_POINT('Ctrl Pts',(19.5770458564908,56.0262125668604,74.7470223626232)) ;
#9469 = CARTESIAN_POINT('Ctrl Pts',(19.9102397208812,55.5885108130449,75.1586127326548)) ;
#9470 = CARTESIAN_POINT('Ctrl Pts',(20.0010453943668,55.586605550614,74.9845706865102)) ;
#9471 = CARTESIAN_POINT('Ctrl Pts',(19.8532587941722,55.4852720162805,74.9044079068786)) ;
#9472 = CARTESIAN_POINT('Ctrl Pts',(20.0560810388402,55.3179011606656,75.231708743013)) ;
#9473 = CARTESIAN_POINT('Ctrl Pts',(20.1432282407444,55.3159940909541,75.055805915533)) ;
#9474 = CARTESIAN_POINT('Ctrl Pts',(19.9938011163935,55.2146518759856,74.9787548834564)) ;
#9475 = CARTESIAN_POINT('Ctrl Pts',(20.352530228535,54.7764805321452,75.3688135322997)) ;
#9476 = CARTESIAN_POINT('Ctrl Pts',(20.4322399575503,54.7745728258514,75.1894144826555)) ;
#9477 = CARTESIAN_POINT('Ctrl Pts',(20.2797798149369,54.673110454093,75.1187172652187)) ;
#9478 = CARTESIAN_POINT('Ctrl Pts',(20.5031363980417,54.5052712784276,75.4327965800233)) ;
#9479 = CARTESIAN_POINT('Ctrl Pts',(20.5790612867906,54.5033650628295,75.2517668182727)) ;
#9480 = CARTESIAN_POINT('Ctrl Pts',(20.4250872640913,54.4020271817646,75.1842528618848)) ;
#9481 = CARTESIAN_POINT('Ctrl Pts',(20.8073844976248,53.963881271126,75.5509243276279)) ;
#9482 = CARTESIAN_POINT('Ctrl Pts',(20.8756702730153,53.9619749130767,75.3668762682082)) ;
#9483 = CARTESIAN_POINT('Ctrl Pts',(20.7190207758772,53.8606102461995,75.305868774962)) ;
#9484 = CARTESIAN_POINT('Ctrl Pts',(20.9613691600088,53.6935003223872,75.6052113061699)) ;
#9485 = CARTESIAN_POINT('Ctrl Pts',(21.0257878867995,53.6915946089085,75.4197734669531)) ;
#9486 = CARTESIAN_POINT('Ctrl Pts',(20.8679145757183,53.5901950776532,75.3620650643573)) ;
#9487 = CARTESIAN_POINT('Ctrl Pts',(21.2722115036904,53.1525885953719,75.7039526161564)) ;
#9488 = CARTESIAN_POINT('Ctrl Pts',(21.3288198886603,53.150683235797,75.5159851220233)) ;
#9489 = CARTESIAN_POINT('Ctrl Pts',(21.168635977305,53.0493503316648,75.4649147748249)) ;
#9490 = CARTESIAN_POINT('Ctrl Pts',(21.4290379841683,52.8821999703398,75.7484084510137)) ;
#9491 = CARTESIAN_POINT('Ctrl Pts',(21.4817073897842,52.8802927777274,75.5592990080604)) ;
#9492 = CARTESIAN_POINT('Ctrl Pts',(21.3204986044484,52.7789455602911,75.5115909288728)) ;
#9493 = CARTESIAN_POINT('Ctrl Pts',(21.7455028833639,52.34155747258,75.8274862850819)) ;
#9494 = CARTESIAN_POINT('Ctrl Pts',(21.7902223538765,52.3396495857205,75.6363372625247)) ;
#9495 = CARTESIAN_POINT('Ctrl Pts',(21.6272322413106,52.2381712237465,75.5954312381129)) ;
#9496 = CARTESIAN_POINT('Ctrl Pts',(21.9050535263985,52.0708923183297,75.8620748678819)) ;
#9497 = CARTESIAN_POINT('Ctrl Pts',(21.9457586711354,52.0689860211318,75.6700346895836)) ;
#9498 = CARTESIAN_POINT('Ctrl Pts',(21.7818685831244,51.9676510264301,75.6325282562937)) ;
#9499 = CARTESIAN_POINT('Ctrl Pts',(22.2260740470942,51.5294526417416,75.921184684073)) ;
#9500 = CARTESIAN_POINT('Ctrl Pts',(22.2587094058815,51.5275461441382,75.7276087174543)) ;
#9501 = CARTESIAN_POINT('Ctrl Pts',(22.0934146827021,51.4261734609838,75.696996712368)) ;
#9502 = CARTESIAN_POINT('Ctrl Pts',(22.3878904045578,51.2584285629873,75.9457535234147)) ;
#9503 = CARTESIAN_POINT('Ctrl Pts',(22.416456657201,51.2565228090173,75.7515349229333)) ;
#9504 = CARTESIAN_POINT('Ctrl Pts',(22.2505651295337,51.1551340723535,75.7243991118759)) ;
#9505 = CARTESIAN_POINT('Ctrl Pts',(22.712114476026,50.7168256229722,75.9845992195019)) ;
#9506 = CARTESIAN_POINT('Ctrl Pts',(22.7325252779384,50.7149201642429,75.7893564712939)) ;
#9507 = CARTESIAN_POINT('Ctrl Pts',(22.5656118445195,50.6135869790189,75.769183509045)) ;
#9508 = CARTESIAN_POINT('Ctrl Pts',(22.8746038558045,50.4462620313528,75.9989086646007)) ;
#9509 = CARTESIAN_POINT('Ctrl Pts',(22.8909288083536,50.4443547062682,75.8032814399391)) ;
#9510 = CARTESIAN_POINT('Ctrl Pts',(22.7236412533748,50.3430015532564,75.7866059993292)) ;
#9511 = CARTESIAN_POINT('Ctrl Pts',(23.200335139236,49.9056099882949,76.0173280779025)) ;
#9512 = CARTESIAN_POINT('Ctrl Pts',(23.2084676499439,49.9037019096726,75.8211857194506)) ;
#9513 = CARTESIAN_POINT('Ctrl Pts',(23.0407104726203,49.8022062837629,75.8115271717256)) ;
#9514 = CARTESIAN_POINT('Ctrl Pts',(23.3634257556432,49.6350408217839,76.0214196212264)) ;
#9515 = CARTESIAN_POINT('Ctrl Pts',(23.3674505868088,49.6331344368352,75.8251542835963)) ;
#9516 = CARTESIAN_POINT('Ctrl Pts',(23.1994351681766,49.5318014383597,75.8190003897153)) ;
#9517 = CARTESIAN_POINT('Ctrl Pts',(23.6894762533187,49.0942250306786,76.0193813810723)) ;
#9518 = CARTESIAN_POINT('Ctrl Pts',(23.6852957248443,49.092318386207,75.8231180356694)) ;
#9519 = CARTESIAN_POINT('Ctrl Pts',(23.5171978570909,48.9909365753488,75.8239920330866)) ;
#9520 = CARTESIAN_POINT('Ctrl Pts',(23.8526613974115,48.8238179925217,76.013242383314)) ;
#9521 = CARTESIAN_POINT('Ctrl Pts',(23.8443723781408,48.8219121926012,75.8171095821339)) ;
#9522 = CARTESIAN_POINT('Ctrl Pts',(23.6763279800096,48.7205331729422,75.821501992585)) ;
#9523 = CARTESIAN_POINT('Ctrl Pts',(24.1782986668665,48.2823982253296,75.9907308384264)) ;
#9524 = CARTESIAN_POINT('Ctrl Pts',(24.1618100373473,48.2804926625387,75.7951178126276)) ;
#9525 = CARTESIAN_POINT('Ctrl Pts',(23.9940710595387,48.1791582422039,75.8065384791858)) ;
#9526 = CARTESIAN_POINT('Ctrl Pts',(24.3408658244874,48.0114576298608,75.9743576213341)) ;
#9527 = CARTESIAN_POINT('Ctrl Pts',(24.3202852562274,48.0095520696295,75.7791284959206)) ;
#9528 = CARTESIAN_POINT('Ctrl Pts',(24.1529117568251,47.9080609643498,75.7940537064683)) ;
#9529 = CARTESIAN_POINT('Ctrl Pts',(24.6648859953999,47.4697670852043,75.9313851632708)) ;
#9530 = CARTESIAN_POINT('Ctrl Pts',(24.6361421055437,47.4678622559149,75.737193617338)) ;
#9531 = CARTESIAN_POINT('Ctrl Pts',(24.4694621780701,47.3665093096488,75.7591266505605)) ;
#9532 = CARTESIAN_POINT('Ctrl Pts',(24.8258807196733,47.1991192501834,75.9048568447549)) ;
#9533 = CARTESIAN_POINT('Ctrl Pts',(24.7930818640022,47.1972127705253,75.7113096559819)) ;
#9534 = CARTESIAN_POINT('Ctrl Pts',(24.6268855561176,47.0958808570305,75.7367272449909)) ;
#9535 = CARTESIAN_POINT('Ctrl Pts',(25.1458531545381,46.6582159321068,75.8417831790114)) ;
#9536 = CARTESIAN_POINT('Ctrl Pts',(25.1049928075486,46.6563091331506,75.6497745295534)) ;
#9537 = CARTESIAN_POINT('Ctrl Pts',(24.9400382258872,46.5549171221349,75.6821115969087)) ;
#9538 = CARTESIAN_POINT('Ctrl Pts',(25.30494646225,46.3878930438263,75.8052019711465)) ;
#9539 = CARTESIAN_POINT('Ctrl Pts',(25.2600759105256,46.3859871917113,75.6140912947864)) ;
#9540 = CARTESIAN_POINT('Ctrl Pts',(25.0958217439246,46.284617201445,75.649875303476)) ;
#9541 = CARTESIAN_POINT('Ctrl Pts',(25.6202833300099,45.8470089936472,75.7222021278697)) ;
#9542 = CARTESIAN_POINT('Ctrl Pts',(25.5674638607462,45.845103318913,75.5331348858038)) ;
#9543 = CARTESIAN_POINT('Ctrl Pts',(25.4048302998281,45.7437666877396,75.575757312238)) ;
#9544 = CARTESIAN_POINT('Ctrl Pts',(25.7766280265348,45.5765948766363,75.6757691159531)) ;
#9545 = CARTESIAN_POINT('Ctrl Pts',(25.719868519592,45.5746876690806,75.4878440205586)) ;
#9546 = CARTESIAN_POINT('Ctrl Pts',(25.5581897868318,45.4732994150165,75.5338518072996)) ;
#9547 = CARTESIAN_POINT('Ctrl Pts',(25.931588121197,45.3060601767044,75.6243964515729)) ;
#9548 = CARTESIAN_POINT('Ctrl Pts',(25.8709204598157,45.3041537286489,75.4377421295873)) ;
#9549 = CARTESIAN_POINT('Ctrl Pts',(25.710296883923,45.2027271666488,75.4871056281043)) ;
#9550 = CARTESIAN_POINT('Ctrl Pts',(26.0863976142602,45.1993067880441,75.5689330654432)) ;
#9551 = CARTESIAN_POINT('Ctrl Pts',(26.0220932596633,45.2022941676425,75.38578662784)) ;
#9552 = CARTESIAN_POINT('Ctrl Pts',(26.1774539338622,45.3026134137914,75.3267467952831)) ;
#9553 = CARTESIAN_POINT('Ctrl Pts',(25.9256608515516,45.4820412744497,75.62601128439)) ;
#9554 = CARTESIAN_POINT('Ctrl Pts',(25.865362711039,45.4850270679879,75.4414566098922)) ;
#9555 = CARTESIAN_POINT('Ctrl Pts',(26.0220178563139,45.5853439255572,75.3858152824602)) ;
#9556 = CARTESIAN_POINT('Ctrl Pts',(25.7634007076745,45.7643410734524,75.677684307806)) ;
#9557 = CARTESIAN_POINT('Ctrl Pts',(25.7071510922706,45.7673274764235,75.4918604580629)) ;
#9558 = CARTESIAN_POINT('Ctrl Pts',(25.8650267437967,45.8675609242127,75.4396377628776)) ;
#9559 = CARTESIAN_POINT('Ctrl Pts',(25.4365228584406,46.3280183067178,75.7701628739833)) ;
#9560 = CARTESIAN_POINT('Ctrl Pts',(25.3884194289408,46.3310049155781,75.5820650392191)) ;
#9561 = CARTESIAN_POINT('Ctrl Pts',(25.5484108731406,46.4312549192326,75.536770822617)) ;
#9562 = CARTESIAN_POINT('Ctrl Pts',(25.2716852659958,46.609335596205,75.8110255869744)) ;
#9563 = CARTESIAN_POINT('Ctrl Pts',(25.227688531219,46.6123217179243,75.6219236471007)) ;
#9564 = CARTESIAN_POINT('Ctrl Pts',(25.3886032840335,46.7126174787231,75.5801309568726)) ;
#9565 = CARTESIAN_POINT('Ctrl Pts',(24.9401111780303,47.1717937445101,75.8818362706009)) ;
#9566 = CARTESIAN_POINT('Ctrl Pts',(24.9043789784248,47.1747789756424,75.6910024575541)) ;
#9567 = CARTESIAN_POINT('Ctrl Pts',(25.0669976654131,47.2750030883893,75.6562349436383)) ;
#9568 = CARTESIAN_POINT('Ctrl Pts',(24.7734305499936,47.4527838881785,75.9117853151364)) ;
#9569 = CARTESIAN_POINT('Ctrl Pts',(24.7418488874936,47.4557718390911,75.7202204583389)) ;
#9570 = CARTESIAN_POINT('Ctrl Pts',(24.9051764209183,47.5560106521802,75.6889957400452)) ;
#9571 = CARTESIAN_POINT('Ctrl Pts',(24.4382874723605,48.0142871287959,75.9608038245404)) ;
#9572 = CARTESIAN_POINT('Ctrl Pts',(24.4150496664146,48.0172768213996,75.768044108176)) ;
#9573 = CARTESIAN_POINT('Ctrl Pts',(24.5795009866196,48.1176560532572,75.7439548245032)) ;
#9574 = CARTESIAN_POINT('Ctrl Pts',(24.269958730186,48.2952668191079,75.9798400629779)) ;
#9575 = CARTESIAN_POINT('Ctrl Pts',(24.250919768841,48.2982535238078,75.7866256771499)) ;
#9576 = CARTESIAN_POINT('Ctrl Pts',(24.4159420948042,48.3984774868592,75.7661011315856)) ;
#9577 = CARTESIAN_POINT('Ctrl Pts',(23.9324843805748,48.8569739450404,76.0069197948193)) ;
#9578 = CARTESIAN_POINT('Ctrl Pts',(23.9218485613817,48.8599612929863,75.8130594689155)) ;
#9579 = CARTESIAN_POINT('Ctrl Pts',(24.0875772524104,48.9602369845976,75.799720427907)) ;
#9580 = CARTESIAN_POINT('Ctrl Pts',(23.7630925057922,49.1378578224385,76.0149733475353)) ;
#9581 = CARTESIAN_POINT('Ctrl Pts',(23.7566759997451,49.1408439739377,75.8209278031086)) ;
#9582 = CARTESIAN_POINT('Ctrl Pts',(23.9226618863959,49.2411084827015,75.8111948341747)) ;
#9583 = CARTESIAN_POINT('Ctrl Pts',(23.4241550653974,49.7002903800858,76.0200135779628)) ;
#9584 = CARTESIAN_POINT('Ctrl Pts',(23.4261790755229,49.703276075074,75.8258737420784)) ;
#9585 = CARTESIAN_POINT('Ctrl Pts',(23.592451809069,49.8035038746523,75.8233630227755)) ;
#9586 = CARTESIAN_POINT('Ctrl Pts',(23.2545251031872,49.9815741041393,76.0170168575449)) ;
#9587 = CARTESIAN_POINT('Ctrl Pts',(23.2607689883619,49.9845603796949,75.8229622257759)) ;
#9588 = CARTESIAN_POINT('Ctrl Pts',(23.4269824796514,50.084920629536,75.8240701185917)) ;
#9589 = CARTESIAN_POINT('Ctrl Pts',(22.9149982686695,50.5452598054651,75.9998797474338)) ;
#9590 = CARTESIAN_POINT('Ctrl Pts',(22.9296979857808,50.5482445256842,75.8062861236819)) ;
#9591 = CARTESIAN_POINT('Ctrl Pts',(23.0957758973726,50.6484794514056,75.8146395997979)) ;
#9592 = CARTESIAN_POINT('Ctrl Pts',(22.7454660608442,50.8275371605747,75.9857636870294)) ;
#9593 = CARTESIAN_POINT('Ctrl Pts',(22.7643842449477,50.8305243023702,75.7925368283109)) ;
#9594 = CARTESIAN_POINT('Ctrl Pts',(22.9302473046794,50.9307473367347,75.8045130352185)) ;
#9595 = CARTESIAN_POINT('Ctrl Pts',(22.4915165114997,51.2516112326304,75.9561999963104)) ;
#9596 = CARTESIAN_POINT('Ctrl Pts',(22.5167536338216,51.2545984104416,75.763729312436)) ;
#9597 = CARTESIAN_POINT('Ctrl Pts',(22.6820674732779,51.3548887142751,75.7811302146028)) ;
#9598 = CARTESIAN_POINT('Ctrl Pts',(22.406841155564,51.3931523912311,75.9449323425022)) ;
#9599 = CARTESIAN_POINT('Ctrl Pts',(22.434185480836,51.3961391935531,75.7527491069979)) ;
#9600 = CARTESIAN_POINT('Ctrl Pts',(22.5992892067911,51.4964465475109,75.77195900654)) ;
#9601 = CARTESIAN_POINT('Ctrl Pts',(22.2380774216862,51.6761627264457,75.919643988823)) ;
#9602 = CARTESIAN_POINT('Ctrl Pts',(22.2696228165867,51.6791488679009,75.7281072912384)) ;
#9603 = CARTESIAN_POINT('Ctrl Pts',(22.4342963723503,51.7794030062205,75.7509296120974)) ;
#9604 = CARTESIAN_POINT('Ctrl Pts',(22.1539868343232,51.8176028378155,75.9056277281354)) ;
#9605 = CARTESIAN_POINT('Ctrl Pts',(22.1876248225326,51.8205891355633,75.7144479277084)) ;
#9606 = CARTESIAN_POINT('Ctrl Pts',(22.3520464638859,51.9208298261597,75.7390706210171)) ;
#9607 = CARTESIAN_POINT('Ctrl Pts',(21.9025850641051,52.2417288193263,75.8594804930087)) ;
#9608 = CARTESIAN_POINT('Ctrl Pts',(21.9424783701571,52.2447151365766,75.6694719008893)) ;
#9609 = CARTESIAN_POINT('Ctrl Pts',(22.1060334622313,52.3449566194381,75.6994758960422)) ;
#9610 = CARTESIAN_POINT('Ctrl Pts',(21.7360305487315,52.5241300049792,75.8232269920363)) ;
#9611 = CARTESIAN_POINT('Ctrl Pts',(21.7800665820217,52.5271161389007,75.6341332124948)) ;
#9612 = CARTESIAN_POINT('Ctrl Pts',(21.9428878891998,52.6274277787848,75.6676973569287)) ;
#9613 = CARTESIAN_POINT('Ctrl Pts',(21.4057304837302,53.0891744812252,75.7399061920707)) ;
#9614 = CARTESIAN_POINT('Ctrl Pts',(21.4579849498291,53.0921595377542,75.552919602523)) ;
#9615 = CARTESIAN_POINT('Ctrl Pts',(21.6192326546544,53.1923844744817,75.5935737756274)) ;
#9616 = CARTESIAN_POINT('Ctrl Pts',(21.2421056534695,53.3716654702888,75.6928812421765)) ;
#9617 = CARTESIAN_POINT('Ctrl Pts',(21.2984281526556,53.3746531995856,75.5070791947283)) ;
#9618 = CARTESIAN_POINT('Ctrl Pts',(21.4587454410097,53.4748857690477,75.5512442980755)) ;
#9619 = CARTESIAN_POINT('Ctrl Pts',(20.9179077319592,53.9365848433119,75.5880960700119)) ;
#9620 = CARTESIAN_POINT('Ctrl Pts',(20.9822904856432,53.9395741566644,75.4049263975121)) ;
#9621 = CARTESIAN_POINT('Ctrl Pts',(21.1404564827692,54.0399343658719,75.4560318818304)) ;
#9622 = CARTESIAN_POINT('Ctrl Pts',(20.7574078709364,54.2194050938411,75.5303438342495)) ;
#9623 = CARTESIAN_POINT('Ctrl Pts',(20.8257847793342,54.2223916877142,75.3486320539804)) ;
#9624 = CARTESIAN_POINT('Ctrl Pts',(20.9828673359832,54.322617765037,75.4032076168567)) ;
#9625 = CARTESIAN_POINT('Ctrl Pts',(20.4404376642166,54.7853172885882,75.4043970887111)) ;
#9626 = CARTESIAN_POINT('Ctrl Pts',(20.5166947213234,54.7883043793635,75.225847521315)) ;
#9627 = CARTESIAN_POINT('Ctrl Pts',(20.6712193285801,54.8885704141613,75.2872321944973)) ;
#9628 = CARTESIAN_POINT('Ctrl Pts',(20.2837973428701,55.0683374452493,75.3361184767196)) ;
#9629 = CARTESIAN_POINT('Ctrl Pts',(20.3639489350762,55.07132357191,75.1592827459495)) ;
#9630 = CARTESIAN_POINT('Ctrl Pts',(20.5170877424361,55.1715968138496,75.2240365555281)) ;
#9631 = CARTESIAN_POINT('Ctrl Pts',(19.9759898322398,55.6338317486207,75.1897533276409)) ;
#9632 = CARTESIAN_POINT('Ctrl Pts',(20.0637929682781,55.636817283455,75.0165911195765)) ;
#9633 = CARTESIAN_POINT('Ctrl Pts',(20.2139803198389,55.7370429277458,75.0879860149741)) ;
#9634 = CARTESIAN_POINT('Ctrl Pts',(19.8246910607917,55.9162154787288,75.1116345999751)) ;
#9635 = CARTESIAN_POINT('Ctrl Pts',(19.9162531085382,55.9192018043292,74.9404246400929)) ;
#9636 = CARTESIAN_POINT('Ctrl Pts',(20.0647700907842,56.0195762764982,75.0150453656116)) ;
#9637 = CARTESIAN_POINT('Ctrl Pts',(19.5271637169588,56.4812254904619,74.9454381365164)) ;
#9638 = CARTESIAN_POINT('Ctrl Pts',(19.6261205413857,56.4842101348273,74.7783984369201)) ;
#9639 = CARTESIAN_POINT('Ctrl Pts',(19.7713027695013,56.5844490941092,74.8594729793997)) ;
#9640 = CARTESIAN_POINT('Ctrl Pts',(19.3813158328695,56.7637439358551,74.8575775464296)) ;
#9641 = CARTESIAN_POINT('Ctrl Pts',(19.4838949469898,56.7667309512119,74.6927382117415)) ;
#9642 = CARTESIAN_POINT('Ctrl Pts',(19.6272799015428,56.8669533046052,74.7769691201447)) ;
#9643 = CARTESIAN_POINT('Ctrl Pts',(19.095442866224,57.3288079962577,74.6723447445499)) ;
#9644 = CARTESIAN_POINT('Ctrl Pts',(19.2051226735476,57.3317959922188,74.5121391388438)) ;
#9645 = CARTESIAN_POINT('Ctrl Pts',(19.3446542775862,57.4320972450331,74.6025284739922)) ;
#9646 = CARTESIAN_POINT('Ctrl Pts',(18.9553476788922,57.6115036704006,74.574907756248)) ;
#9647 = CARTESIAN_POINT('Ctrl Pts',(19.0685079296873,57.6144899220291,74.4171434179548)) ;
#9648 = CARTESIAN_POINT('Ctrl Pts',(19.206054842789,57.7147356136766,74.5105810395141)) ;
#9649 = CARTESIAN_POINT('Ctrl Pts',(18.6818459265001,58.1775332618958,74.3710420390506)) ;
#9650 = CARTESIAN_POINT('Ctrl Pts',(18.8017978488122,58.1805194049365,74.2183781834203)) ;
#9651 = CARTESIAN_POINT('Ctrl Pts',(18.9351306118037,58.2807563670214,74.3177449426027)) ;
#9652 = CARTESIAN_POINT('Ctrl Pts',(18.5483121501979,58.4605262973907,74.2645110032067)) ;
#9653 = CARTESIAN_POINT('Ctrl Pts',(18.6715801956769,58.463511044069,74.1145080753123)) ;
#9654 = CARTESIAN_POINT('Ctrl Pts',(18.8026553177914,58.563858734355,74.2167324991218)) ;
#9655 = CARTESIAN_POINT('Ctrl Pts',(18.4187092424426,58.7433256931628,74.1539683873054)) ;
#9656 = CARTESIAN_POINT('Ctrl Pts',(18.5451935747115,58.7463119239391,74.006735167518)) ;
#9657 = CARTESIAN_POINT('Ctrl Pts',(18.6740364880035,58.846513767945,74.1118252195922)) ;
#9658 = CARTESIAN_POINT('',(0.,0.,0.)) ;
#9659 = CARTESIAN_POINT('Origin',(23.47768801576,48.8830586252741,68.2224337400009)) ;
#9660 = CARTESIAN_POINT('',(59.22768801576,48.8830586252741,68.2224337400009)) ;
#9661 = CARTESIAN_POINT('Origin',(23.47768801576,48.8830586252741,68.2224337400009)) ;
#9662 = CARTESIAN_POINT('',(59.22768801576,58.8830586252741,68.2224337400009)) ;
#9663 = CARTESIAN_POINT('',(59.22768801576,48.8830586252741,68.2224337400009)) ;
#9664 = CARTESIAN_POINT('Origin',(23.47768801576,58.8830586252741,68.2224337400009)) ;
#9665 = CARTESIAN_POINT('Origin',(23.47768801576,48.8830586252741,68.2224337400009)) ;
#9666 = CARTESIAN_POINT('',(59.37768801576,58.8830586252741,68.2224337400009)) ;
#9667 = CARTESIAN_POINT('Origin',(23.47768801576,58.8830586252741,68.2224337400009)) ;
#9668 = CARTESIAN_POINT('',(59.37768801576,48.8830586252741,68.2224337400009)) ;
#9669 = CARTESIAN_POINT('',(59.37768801576,48.8830586252741,68.2224337400009)) ;
#9670 = CARTESIAN_POINT('Origin',(23.47768801576,48.8830586252741,68.2224337400009)) ;
#9671 = CARTESIAN_POINT('Origin',(23.47768801576,48.8830586252741,68.2224337400009)) ;
#9672 = CARTESIAN_POINT('Origin',(23.47768801576,58.8830586252741,68.2224337400009)) ;
#9673 = CARTESIAN_POINT('',(0.,0.,0.)) ;
#9674 = CARTESIAN_POINT('Origin',(17.47768801576,59.8830586252739,62.222433740001)) ;
#9675 = CARTESIAN_POINT('',(17.47768801576,66.8830586252738,72.2224337400011)) ;
#9676 = CARTESIAN_POINT('',(17.47768801576,66.8830586252739,64.2224337400011)) ;
#9677 = CARTESIAN_POINT('',(17.47768801576,66.8830586252739,62.2224337400011)) ;
#9678 = CARTESIAN_POINT('',(17.47768801576,59.8830586252739,64.2224337400011)) ;
#9679 = CARTESIAN_POINT('',(17.47768801576,59.8830586252739,64.2224337400011)) ;
#9680 = CARTESIAN_POINT('',(17.47768801576,59.8830586252738,72.222433740001)) ;
#9681 = CARTESIAN_POINT('',(17.47768801576,59.8830586252739,62.222433740001)) ;
#9682 = CARTESIAN_POINT('',(17.47768801576,59.8830586252738,72.222433740001)) ;
#9683 = CARTESIAN_POINT('Origin',(29.47768801576,59.8830586252739,62.222433740001)) ;
#9684 = CARTESIAN_POINT('',(19.47768801576,66.8830586252739,62.2224337400011)) ;
#9685 = CARTESIAN_POINT('',(27.47768801576,66.8830586252739,62.2224337400011)) ;
#9686 = CARTESIAN_POINT('',(29.47768801576,66.8830586252739,62.2224337400011)) ;
#9687 = CARTESIAN_POINT('',(27.47768801576,59.8830586252739,62.222433740001)) ;
#9688 = CARTESIAN_POINT('',(27.4776880157599,59.8830586252739,62.222433740001)) ;
#9689 = CARTESIAN_POINT('',(19.47768801576,59.8830586252739,62.222433740001)) ;
#9690 = CARTESIAN_POINT('',(29.47768801576,59.8830586252739,62.222433740001)) ;
#9691 = CARTESIAN_POINT('',(19.47768801576,59.8830586252739,62.222433740001)) ;
#9692 = CARTESIAN_POINT('Origin',(29.47768801576,59.8830586252739,62.222433740001)) ;
#9693 = CARTESIAN_POINT('',(29.47768801576,59.8830586252739,64.2224337400011)) ;
#9694 = CARTESIAN_POINT('',(29.47768801576,59.8830586252738,72.2224337400011)) ;
#9695 = CARTESIAN_POINT('',(29.47768801576,59.8830586252739,62.222433740001)) ;
#9696 = CARTESIAN_POINT('',(29.47768801576,66.8830586252739,64.2224337400011)) ;
#9697 = CARTESIAN_POINT('',(29.47768801576,59.8830586252739,64.2224337400011)) ;
#9698 = CARTESIAN_POINT('',(29.47768801576,66.8830586252738,72.2224337400011)) ;
#9699 = CARTESIAN_POINT('',(29.47768801576,66.8830586252739,62.2224337400011)) ;
#9700 = CARTESIAN_POINT('',(29.47768801576,59.8830586252738,72.2224337400011)) ;
#9701 = CARTESIAN_POINT('Origin',(29.47768801576,59.8830586252738,74.2224337400011)) ;
#9702 = CARTESIAN_POINT('',(27.4776880157599,66.8830586252738,74.2224337400011)) ;
#9703 = CARTESIAN_POINT('',(19.47768801576,66.8830586252738,74.2224337400011)) ;
#9704 = CARTESIAN_POINT('',(29.47768801576,66.8830586252738,74.2224337400011)) ;
#9705 = CARTESIAN_POINT('',(19.47768801576,59.8830586252738,74.2224337400011)) ;
#9706 = CARTESIAN_POINT('',(19.47768801576,59.8830586252738,74.2224337400011)) ;
#9707 = CARTESIAN_POINT('',(27.4776880157599,59.8830586252738,74.2224337400011)) ;
#9708 = CARTESIAN_POINT('',(29.47768801576,59.8830586252738,74.2224337400011)) ;
#9709 = CARTESIAN_POINT('',(27.4776880157599,59.8830586252738,74.2224337400011)) ;
#9710 = CARTESIAN_POINT('Origin',(23.47768801576,59.8830586252739,68.2224337400011)) ;
#9711 = CARTESIAN_POINT('Origin',(27.4776880157599,59.8830586252739,64.2224337400011)) ;
#9712 = CARTESIAN_POINT('Origin',(27.4776880157599,59.8830586252738,72.222433740001)) ;
#9713 = CARTESIAN_POINT('Origin',(19.47768801576,59.8830586252738,72.222433740001)) ;
#9714 = CARTESIAN_POINT('Origin',(19.47768801576,59.8830586252739,64.2224337400011)) ;
#9715 = CARTESIAN_POINT('Origin',(23.47768801576,66.8830586252739,68.2224337400011)) ;
#9716 = CARTESIAN_POINT('Origin',(27.4776880157599,66.8830586252739,64.2224337400011)) ;
#9717 = CARTESIAN_POINT('Origin',(19.47768801576,66.8830586252739,64.2224337400011)) ;
#9718 = CARTESIAN_POINT('Origin',(19.47768801576,66.8830586252738,72.2224337400011)) ;
#9719 = CARTESIAN_POINT('Origin',(27.4776880157599,66.8830586252738,72.2224337400011)) ;
#9720 = CARTESIAN_POINT('Origin',(27.4776880157599,59.8830586252739,64.2224337400011)) ;
#9721 = CARTESIAN_POINT('Origin',(19.47768801576,59.8830586252739,64.2224337400011)) ;
#9722 = CARTESIAN_POINT('Origin',(19.47768801576,59.8830586252738,72.222433740001)) ;
#9723 = CARTESIAN_POINT('Origin',(27.4776880157599,59.8830586252738,72.222433740001)) ;
#9724 = CARTESIAN_POINT('',(0.,0.,0.)) ;
#9725 = CARTESIAN_POINT('',(0.,0.,0.)) ;
#9726 = CARTESIAN_POINT('',(0.,0.,0.)) ;
#9727 = CARTESIAN_POINT('',(0.,0.,0.)) ;
#9728 = CARTESIAN_POINT('',(0.,0.,0.)) ;
#9729 = CARTESIAN_POINT('Origin',(23.47768801576,41.8330586252738,68.2224337399912)) ;
#9730 = CARTESIAN_POINT('',(-17.5327992399109,40.9830586252738,68.2224337399912)) ;
#9731 = CARTESIAN_POINT('Origin',(23.47768801576,40.9830586252738,68.2224337399912)) ;
#9732 = CARTESIAN_POINT('',(-17.5327992399109,40.8330586252738,68.2224337399912)) ;
#9733 = CARTESIAN_POINT('',(-17.5327992399108,41.8330586252738,68.2224337399912)) ;
#9734 = CARTESIAN_POINT('Origin',(23.47768801576,40.8330586252738,68.2224337399912)) ;
#9735 = CARTESIAN_POINT('Origin',(23.47768801576,40.9830586252738,68.222433740001)) ;
#9736 = CARTESIAN_POINT('',(65.42768801576,40.983058625274,28.272433740001)) ;
#9737 = CARTESIAN_POINT('',(65.42768801576,40.9830586252737,108.172433740001)) ;
#9738 = CARTESIAN_POINT('',(65.42768801576,40.983058625274,26.272433740001)) ;
#9739 = CARTESIAN_POINT('',(63.42768801576,40.983058625274,26.272433740001)) ;
#9740 = CARTESIAN_POINT('',(63.42768801576,40.983058625274,26.272433740001)) ;
#9741 = CARTESIAN_POINT('',(-16.47231198424,40.983058625274,26.272433740001)) ;
#9742 = CARTESIAN_POINT('',(65.42768801576,40.983058625274,26.272433740001)) ;
#9743 = CARTESIAN_POINT('',(-18.47231198424,40.983058625274,28.272433740001)) ;
#9744 = CARTESIAN_POINT('',(-18.47231198424,40.983058625274,28.272433740001)) ;
#9745 = CARTESIAN_POINT('',(-18.47231198424,40.9830586252737,108.172433740001)) ;
#9746 = CARTESIAN_POINT('',(-18.47231198424,40.983058625274,26.272433740001)) ;
#9747 = CARTESIAN_POINT('',(-16.47231198424,40.9830586252737,110.172433740001)) ;
#9748 = CARTESIAN_POINT('',(-16.47231198424,40.9830586252737,110.172433740001)) ;
#9749 = CARTESIAN_POINT('',(63.4276880157599,40.9830586252737,110.172433740001)) ;
#9750 = CARTESIAN_POINT('',(65.42768801576,40.9830586252737,110.172433740001)) ;
#9751 = CARTESIAN_POINT('',(65.42768801576,40.9830586252737,108.172433740001)) ;
#9752 = CARTESIAN_POINT('Origin',(23.47768801576,40.8330586252738,68.222433740001)) ;
#9753 = CARTESIAN_POINT('',(-16.47231198424,40.833058625274,26.272433740001)) ;
#9754 = CARTESIAN_POINT('',(63.42768801576,40.833058625274,26.272433740001)) ;
#9755 = CARTESIAN_POINT('',(65.42768801576,40.833058625274,26.272433740001)) ;
#9756 = CARTESIAN_POINT('',(65.42768801576,40.833058625274,28.272433740001)) ;
#9757 = CARTESIAN_POINT('',(64.4276880157599,40.833058625274,27.272433740001)) ;
#9758 = CARTESIAN_POINT('',(65.42768801576,40.8330586252737,108.172433740001)) ;
#9759 = CARTESIAN_POINT('',(65.42768801576,40.833058625274,26.272433740001)) ;
#9760 = CARTESIAN_POINT('',(63.4276880157599,40.8330586252737,110.172433740001)) ;
#9761 = CARTESIAN_POINT('',(64.4276880157598,40.8330586252737,109.172433740001)) ;
#9762 = CARTESIAN_POINT('',(-16.47231198424,40.8330586252737,110.172433740001)) ;
#9763 = CARTESIAN_POINT('',(65.42768801576,40.8330586252737,110.172433740001)) ;
#9764 = CARTESIAN_POINT('',(-18.47231198424,40.8330586252737,108.172433740001)) ;
#9765 = CARTESIAN_POINT('',(-17.47231198424,40.8330586252737,109.172433740001)) ;
#9766 = CARTESIAN_POINT('',(-18.47231198424,40.833058625274,28.272433740001)) ;
#9767 = CARTESIAN_POINT('',(-18.47231198424,40.833058625274,26.272433740001)) ;
#9768 = CARTESIAN_POINT('',(-17.47231198424,40.833058625274,27.272433740001)) ;
#9769 = CARTESIAN_POINT('Origin',(63.42768801576,40.983058625274,26.272433740001)) ;
#9770 = CARTESIAN_POINT('',(65.42768801576,40.983058625274,28.272433740001)) ;
#9771 = CARTESIAN_POINT('',(63.42768801576,40.983058625274,26.272433740001)) ;
#9772 = CARTESIAN_POINT('Origin',(-18.47231198424,40.983058625274,28.272433740001)) ;
#9773 = CARTESIAN_POINT('',(-16.47231198424,40.983058625274,26.272433740001)) ;
#9774 = CARTESIAN_POINT('',(-18.47231198424,40.983058625274,28.272433740001)) ;
#9775 = CARTESIAN_POINT('Origin',(-16.47231198424,40.9830586252737,110.172433740001)) ;
#9776 = CARTESIAN_POINT('',(-18.47231198424,40.9830586252737,108.172433740001)) ;
#9777 = CARTESIAN_POINT('',(-16.47231198424,40.9830586252737,110.172433740001)) ;
#9778 = CARTESIAN_POINT('Origin',(65.42768801576,40.9830586252737,108.172433740001)) ;
#9779 = CARTESIAN_POINT('',(63.4276880157599,40.9830586252737,110.172433740001)) ;
#9780 = CARTESIAN_POINT('',(65.42768801576,40.9830586252737,108.172433740001)) ;
#9781 = CARTESIAN_POINT('Origin',(-16.47231198424,41.3830586252737,110.172433740001)) ;
#9782 = CARTESIAN_POINT('',(-16.47231198424,41.3830586252737,110.572433740001)) ;
#9783 = CARTESIAN_POINT('',(-16.47231198424,41.3830586252737,110.722433740001)) ;
#9784 = CARTESIAN_POINT('',(-16.47231198424,41.3830586252737,110.722433740001)) ;
#9785 = CARTESIAN_POINT('Origin',(-16.47231198424,41.3830586252737,110.172433740001)) ;
#9786 = CARTESIAN_POINT('Origin',(-16.47231198424,41.3830586252737,110.172433740001)) ;
#9787 = CARTESIAN_POINT('Origin',(63.4276880157599,41.3830586252737,110.172433740001)) ;
#9788 = CARTESIAN_POINT('',(63.4276880157599,41.3830586252737,110.572433740001)) ;
#9789 = CARTESIAN_POINT('Origin',(63.4276880157599,41.3830586252737,110.172433740001)) ;
#9790 = CARTESIAN_POINT('',(63.4276880157599,41.3830586252737,110.722433740001)) ;
#9791 = CARTESIAN_POINT('',(63.4276880157599,41.3830586252737,110.572433740001)) ;
#9792 = CARTESIAN_POINT('Origin',(63.4276880157599,41.3830586252737,110.172433740001)) ;
#9793 = CARTESIAN_POINT('Origin',(63.4276880157599,41.3830586252737,110.172433740001)) ;
#9794 = CARTESIAN_POINT('',(-16.47231198424,41.3830586252737,110.722433740001)) ;
#9795 = CARTESIAN_POINT('Origin',(63.4276880157599,41.3830586252737,110.172433740001)) ;
#9796 = CARTESIAN_POINT('',(-16.47231198424,41.3830586252737,110.572433740001)) ;
#9797 = CARTESIAN_POINT('Origin',(63.4276880157599,43.3330586252737,110.722433740001)) ;
#9798 = CARTESIAN_POINT('',(63.4276880157599,43.3330586252737,110.572433740001)) ;
#9799 = CARTESIAN_POINT('',(63.4276880157599,43.3330586252737,110.572433740001)) ;
#9800 = CARTESIAN_POINT('',(63.4276880157599,43.3330586252737,110.722433740001)) ;
#9801 = CARTESIAN_POINT('',(63.4276880157599,43.3330586252737,110.722433740001)) ;
#9802 = CARTESIAN_POINT('',(63.4276880157599,40.8330586252736,110.722433740001)) ;
#9803 = CARTESIAN_POINT('Origin',(-16.47231198424,40.9830586252737,110.722433740001)) ;
#9804 = CARTESIAN_POINT('',(-16.47231198424,43.3330586252737,110.722433740001)) ;
#9805 = CARTESIAN_POINT('',(-16.47231198424,40.8330586252736,110.722433740001)) ;
#9806 = CARTESIAN_POINT('',(-16.47231198424,43.3330586252737,110.572433740001)) ;
#9807 = CARTESIAN_POINT('',(-16.47231198424,43.3330586252737,110.722433740001)) ;
#9808 = CARTESIAN_POINT('',(-16.47231198424,40.9830586252737,110.572433740001)) ;
#9809 = CARTESIAN_POINT('Origin',(23.4776880157599,40.8330586252736,110.722433740001)) ;
#9810 = CARTESIAN_POINT('',(23.4776880157599,43.3330586252737,110.722433740001)) ;
#9811 = CARTESIAN_POINT('Origin',(23.4776880157599,40.8330586252736,110.572433740001)) ;
#9812 = CARTESIAN_POINT('',(-16.47231198424,43.3330586252737,110.572433740001)) ;
#9813 = CARTESIAN_POINT('Origin',(-16.47231198424,43.3330586252737,110.722433740001)) ;
#9814 = CARTESIAN_POINT('Origin',(65.42768801576,41.3830586252737,108.172433740001)) ;
#9815 = CARTESIAN_POINT('',(65.82768801576,41.3830586252737,108.172433740001)) ;
#9816 = CARTESIAN_POINT('',(65.97768801576,41.3830586252737,108.172433740001)) ;
#9817 = CARTESIAN_POINT('',(65.97768801576,41.3830586252737,108.172433740001)) ;
#9818 = CARTESIAN_POINT('Origin',(65.42768801576,41.3830586252737,108.172433740001)) ;
#9819 = CARTESIAN_POINT('Origin',(65.42768801576,41.3830586252737,108.172433740001)) ;
#9820 = CARTESIAN_POINT('Origin',(65.42768801576,41.383058625274,28.272433740001)) ;
#9821 = CARTESIAN_POINT('',(65.82768801576,41.383058625274,28.272433740001)) ;
#9822 = CARTESIAN_POINT('Origin',(65.42768801576,41.383058625274,28.272433740001)) ;
#9823 = CARTESIAN_POINT('',(65.97768801576,41.383058625274,28.272433740001)) ;
#9824 = CARTESIAN_POINT('',(65.82768801576,41.383058625274,28.272433740001)) ;
#9825 = CARTESIAN_POINT('Origin',(65.42768801576,41.383058625274,28.272433740001)) ;
#9826 = CARTESIAN_POINT('Origin',(65.42768801576,41.383058625274,28.272433740001)) ;
#9827 = CARTESIAN_POINT('',(65.97768801576,41.3830586252737,108.172433740001)) ;
#9828 = CARTESIAN_POINT('Origin',(65.42768801576,41.383058625274,28.272433740001)) ;
#9829 = CARTESIAN_POINT('',(65.82768801576,41.3830586252737,108.172433740001)) ;
#9830 = CARTESIAN_POINT('Origin',(65.97768801576,43.333058625274,28.272433740001)) ;
#9831 = CARTESIAN_POINT('',(65.82768801576,43.333058625274,28.272433740001)) ;
#9832 = CARTESIAN_POINT('',(65.82768801576,43.333058625274,28.272433740001)) ;
#9833 = CARTESIAN_POINT('',(65.97768801576,43.333058625274,28.272433740001)) ;
#9834 = CARTESIAN_POINT('',(65.97768801576,43.333058625274,28.272433740001)) ;
#9835 = CARTESIAN_POINT('',(65.97768801576,40.8330586252739,28.272433740001)) ;
#9836 = CARTESIAN_POINT('Origin',(65.97768801576,40.9830586252737,108.172433740001)) ;
#9837 = CARTESIAN_POINT('',(65.97768801576,43.3330586252737,108.172433740001)) ;
#9838 = CARTESIAN_POINT('',(65.97768801576,40.8330586252736,108.172433740001)) ;
#9839 = CARTESIAN_POINT('',(65.82768801576,43.3330586252737,108.172433740001)) ;
#9840 = CARTESIAN_POINT('',(65.97768801576,43.3330586252737,108.172433740001)) ;
#9841 = CARTESIAN_POINT('',(65.82768801576,40.9830586252737,108.172433740001)) ;
#9842 = CARTESIAN_POINT('Origin',(65.97768801576,40.8330586252737,68.222433740001)) ;
#9843 = CARTESIAN_POINT('',(65.97768801576,43.3330586252738,68.222433740001)) ;
#9844 = CARTESIAN_POINT('Origin',(65.82768801576,40.8330586252737,68.222433740001)) ;
#9845 = CARTESIAN_POINT('',(65.82768801576,43.3330586252737,108.172433740001)) ;
#9846 = CARTESIAN_POINT('Origin',(65.97768801576,43.3330586252737,108.172433740001)) ;
#9847 = CARTESIAN_POINT('Origin',(63.42768801576,41.383058625274,26.272433740001)) ;
#9848 = CARTESIAN_POINT('',(63.42768801576,41.383058625274,25.872433740001)) ;
#9849 = CARTESIAN_POINT('',(63.42768801576,41.383058625274,25.722433740001)) ;
#9850 = CARTESIAN_POINT('',(63.42768801576,41.383058625274,25.722433740001)) ;
#9851 = CARTESIAN_POINT('Origin',(63.42768801576,41.383058625274,26.272433740001)) ;
#9852 = CARTESIAN_POINT('Origin',(63.42768801576,41.383058625274,26.272433740001)) ;
#9853 = CARTESIAN_POINT('Origin',(-16.47231198424,41.383058625274,26.272433740001)) ;
#9854 = CARTESIAN_POINT('',(-16.47231198424,41.383058625274,25.872433740001)) ;
#9855 = CARTESIAN_POINT('Origin',(-16.47231198424,41.383058625274,26.272433740001)) ;
#9856 = CARTESIAN_POINT('',(-16.47231198424,41.383058625274,25.722433740001)) ;
#9857 = CARTESIAN_POINT('',(-16.47231198424,41.383058625274,25.872433740001)) ;
#9858 = CARTESIAN_POINT('Origin',(-16.47231198424,41.383058625274,26.272433740001)) ;
#9859 = CARTESIAN_POINT('Origin',(-16.47231198424,41.383058625274,26.272433740001)) ;
#9860 = CARTESIAN_POINT('',(63.42768801576,41.383058625274,25.722433740001)) ;
#9861 = CARTESIAN_POINT('Origin',(-16.47231198424,41.383058625274,26.272433740001)) ;
#9862 = CARTESIAN_POINT('',(63.42768801576,41.383058625274,25.872433740001)) ;
#9863 = CARTESIAN_POINT('Origin',(-16.47231198424,43.333058625274,25.722433740001)) ;
#9864 = CARTESIAN_POINT('',(-16.47231198424,43.333058625274,25.872433740001)) ;
#9865 = CARTESIAN_POINT('',(-16.47231198424,43.333058625274,25.872433740001)) ;
#9866 = CARTESIAN_POINT('',(-16.47231198424,43.333058625274,25.722433740001)) ;
#9867 = CARTESIAN_POINT('',(-16.47231198424,43.333058625274,25.722433740001)) ;
#9868 = CARTESIAN_POINT('',(-16.47231198424,40.8330586252739,25.722433740001)) ;
#9869 = CARTESIAN_POINT('Origin',(63.42768801576,40.983058625274,25.722433740001)) ;
#9870 = CARTESIAN_POINT('',(63.42768801576,43.333058625274,25.722433740001)) ;
#9871 = CARTESIAN_POINT('',(63.42768801576,40.8330586252739,25.722433740001)) ;
#9872 = CARTESIAN_POINT('',(63.42768801576,43.333058625274,25.872433740001)) ;
#9873 = CARTESIAN_POINT('',(63.42768801576,43.333058625274,25.722433740001)) ;
#9874 = CARTESIAN_POINT('',(63.42768801576,40.983058625274,25.872433740001)) ;
#9875 = CARTESIAN_POINT('Origin',(23.47768801576,40.8330586252739,25.722433740001)) ;
#9876 = CARTESIAN_POINT('',(23.47768801576,43.333058625274,25.722433740001)) ;
#9877 = CARTESIAN_POINT('Origin',(23.47768801576,40.8330586252739,25.872433740001)) ;
#9878 = CARTESIAN_POINT('',(63.42768801576,43.333058625274,25.872433740001)) ;
#9879 = CARTESIAN_POINT('Origin',(63.42768801576,43.333058625274,25.722433740001)) ;
#9880 = CARTESIAN_POINT('Origin',(-18.47231198424,41.383058625274,28.272433740001)) ;
#9881 = CARTESIAN_POINT('',(-18.87231198424,41.383058625274,28.272433740001)) ;
#9882 = CARTESIAN_POINT('',(-19.02231198424,41.383058625274,28.272433740001)) ;
#9883 = CARTESIAN_POINT('',(-19.02231198424,41.383058625274,28.272433740001)) ;
#9884 = CARTESIAN_POINT('Origin',(-18.47231198424,41.383058625274,28.272433740001)) ;
#9885 = CARTESIAN_POINT('Origin',(-18.47231198424,41.383058625274,28.272433740001)) ;
#9886 = CARTESIAN_POINT('Origin',(-18.47231198424,41.3830586252737,108.172433740001)) ;
#9887 = CARTESIAN_POINT('',(-18.87231198424,41.3830586252737,108.172433740001)) ;
#9888 = CARTESIAN_POINT('Origin',(-18.47231198424,41.3830586252737,108.172433740001)) ;
#9889 = CARTESIAN_POINT('',(-19.02231198424,41.3830586252737,108.172433740001)) ;
#9890 = CARTESIAN_POINT('',(-18.87231198424,41.3830586252737,108.172433740001)) ;
#9891 = CARTESIAN_POINT('Origin',(-18.47231198424,41.3830586252737,108.172433740001)) ;
#9892 = CARTESIAN_POINT('Origin',(-18.47231198424,41.3830586252737,108.172433740001)) ;
#9893 = CARTESIAN_POINT('',(-19.02231198424,41.383058625274,28.272433740001)) ;
#9894 = CARTESIAN_POINT('Origin',(-18.47231198424,41.3830586252737,108.172433740001)) ;
#9895 = CARTESIAN_POINT('',(-18.87231198424,41.383058625274,28.272433740001)) ;
#9896 = CARTESIAN_POINT('Origin',(-19.02231198424,43.3330586252737,108.172433740001)) ;
#9897 = CARTESIAN_POINT('',(-18.87231198424,43.3330586252737,108.172433740001)) ;
#9898 = CARTESIAN_POINT('',(-18.87231198424,43.3330586252737,108.172433740001)) ;
#9899 = CARTESIAN_POINT('',(-19.02231198424,43.3330586252737,108.172433740001)) ;
#9900 = CARTESIAN_POINT('',(-19.02231198424,43.3330586252737,108.172433740001)) ;
#9901 = CARTESIAN_POINT('',(-19.02231198424,40.8330586252736,108.172433740001)) ;
#9902 = CARTESIAN_POINT('Origin',(-19.02231198424,40.983058625274,28.272433740001)) ;
#9903 = CARTESIAN_POINT('',(-19.02231198424,43.333058625274,28.272433740001)) ;
#9904 = CARTESIAN_POINT('',(-19.02231198424,40.8330586252739,28.272433740001)) ;
#9905 = CARTESIAN_POINT('',(-18.87231198424,43.333058625274,28.272433740001)) ;
#9906 = CARTESIAN_POINT('',(-19.02231198424,43.333058625274,28.272433740001)) ;
#9907 = CARTESIAN_POINT('',(-18.87231198424,40.983058625274,28.272433740001)) ;
#9908 = CARTESIAN_POINT('Origin',(-19.02231198424,40.8330586252737,68.222433740001)) ;
#9909 = CARTESIAN_POINT('',(-19.02231198424,43.3330586252738,68.222433740001)) ;
#9910 = CARTESIAN_POINT('Origin',(-18.87231198424,40.8330586252737,68.222433740001)) ;
#9911 = CARTESIAN_POINT('',(-18.87231198424,43.333058625274,28.272433740001)) ;
#9912 = CARTESIAN_POINT('Origin',(-19.02231198424,43.333058625274,28.272433740001)) ;
#9913 = CARTESIAN_POINT('',(0.,0.,0.)) ;
#9914 = CARTESIAN_POINT('Origin',(58.7276880157606,67.0830586252741,67.2224337400009)) ;
#9915 = CARTESIAN_POINT('',(58.7276880157606,67.9830586252741,67.2224337400009)) ;
#9916 = CARTESIAN_POINT('Origin',(58.7276880157606,68.5830586252741,67.2224337400009)) ;
#9917 = CARTESIAN_POINT('',(59.6276880157606,67.0830586252741,67.2224337400009)) ;
#9918 = CARTESIAN_POINT('Origin',(58.7276880157606,67.0830586252741,67.2224337400009)) ;
#9919 = CARTESIAN_POINT('',(60.2276880157606,67.0830586252741,66.6224337400009)) ;
#9920 = CARTESIAN_POINT('Origin',(60.2276880157606,67.0830586252741,67.2224337400009)) ;
#9921 = CARTESIAN_POINT('Origin',(60.2276880157606,67.0830586252741,67.2224337400009)) ;
#9922 = CARTESIAN_POINT('Origin',(40.5810116473826,66.5830586252741,67.2224337400009)) ;
#9923 = CARTESIAN_POINT('',(40.1013291642416,67.8983170467897,67.2224337400009)) ;
#9924 = CARTESIAN_POINT('Origin',(39.8957509571812,68.4619992274392,67.2224337400009)) ;
#9925 = CARTESIAN_POINT('',(40.5810116473826,67.9830586252741,67.2224337400009)) ;
#9926 = CARTESIAN_POINT('Origin',(40.5810116473826,66.5830586252741,67.2224337400009)) ;
#9927 = CARTESIAN_POINT('Origin',(40.5810116473826,68.5830586252741,67.2224337400009)) ;
#9928 = CARTESIAN_POINT('Origin',(31.3743643841387,67.4830586252741,67.2224337400009)) ;
#9929 = CARTESIAN_POINT('',(31.3743643841387,65.4830586252741,66.6224337400009)) ;
#9930 = CARTESIAN_POINT('',(31.3743643841387,66.0830586252741,67.2224337400009)) ;
#9931 = CARTESIAN_POINT('Origin',(31.3743643841387,65.4830586252741,67.2224337400009)) ;
#9932 = CARTESIAN_POINT('Origin',(31.3743643841387,65.4830586252741,67.2224337400009)) ;
#9933 = CARTESIAN_POINT('',(31.8540468672797,66.1678002037585,67.2224337400009)) ;
#9934 = CARTESIAN_POINT('Origin',(31.3743643841387,67.4830586252741,67.2224337400009)) ;
#9935 = CARTESIAN_POINT('',(32.2652032814005,65.0404358424594,67.2224337400009)) ;
#9936 = CARTESIAN_POINT('Origin',(32.0596250743401,65.604118023109,67.2224337400009)) ;
#9937 = CARTESIAN_POINT('Origin',(32.0596250743401,65.604118023109,67.2224337400009)) ;
#9938 = CARTESIAN_POINT('Origin',(30.7276880157606,65.4830586252741,68.2224337400009)) ;
#9939 = CARTESIAN_POINT('',(30.7276880157606,65.4830586252741,66.6224337400009)) ;
#9940 = CARTESIAN_POINT('',(30.7276880157606,65.4830586252741,67.8224337400009)) ;
#9941 = CARTESIAN_POINT('Origin',(30.7276880157606,65.4830586252741,67.2224337400009)) ;
#9942 = CARTESIAN_POINT('',(30.7276880157606,65.4830586252741,68.6224337400009)) ;
#9943 = CARTESIAN_POINT('Origin',(30.7276880157606,65.4830586252741,68.2224337400009)) ;
#9944 = CARTESIAN_POINT('',(30.7276880157606,65.4830586252741,69.8224337400008)) ;
#9945 = CARTESIAN_POINT('Origin',(30.7276880157606,65.4830586252741,69.2224337400009)) ;
#9946 = CARTESIAN_POINT('Origin',(30.7276880157606,65.4830586252741,69.2224337400009)) ;
#9947 = CARTESIAN_POINT('Origin',(30.7276880157606,65.4830586252741,67.2224337400009)) ;
#9948 = CARTESIAN_POINT('Origin',(60.2276880157606,56.5830586252741,68.2224337400009)) ;
#9949 = CARTESIAN_POINT('',(60.2276880157606,56.5830586252741,66.6224337400009)) ;
#9950 = CARTESIAN_POINT('',(60.2276880157606,56.5830586252741,67.8224337400009)) ;
#9951 = CARTESIAN_POINT('Origin',(60.2276880157606,56.5830586252741,67.2224337400009)) ;
#9952 = CARTESIAN_POINT('Origin',(60.2276880157606,56.5830586252741,67.2224337400009)) ;
#9953 = CARTESIAN_POINT('',(60.2276880157606,56.5830586252741,68.6224337400009)) ;
#9954 = CARTESIAN_POINT('Origin',(60.2276880157606,56.5830586252741,68.2224337400009)) ;
#9955 = CARTESIAN_POINT('',(60.2276880157606,56.5830586252741,69.8224337400008)) ;
#9956 = CARTESIAN_POINT('Origin',(60.2276880157606,56.5830586252741,69.2224337400009)) ;
#9957 = CARTESIAN_POINT('Origin',(60.2276880157606,56.5830586252741,69.2224337400009)) ;
#9958 = CARTESIAN_POINT('Origin',(58.7276880157606,67.0830586252741,69.2224337400009)) ;
#9959 = CARTESIAN_POINT('',(60.2276880157606,67.0830586252741,69.8224337400008)) ;
#9960 = CARTESIAN_POINT('',(59.6276880157606,67.0830586252741,69.2224337400009)) ;
#9961 = CARTESIAN_POINT('Origin',(60.2276880157606,67.0830586252741,69.2224337400009)) ;
#9962 = CARTESIAN_POINT('Origin',(60.2276880157606,67.0830586252741,69.2224337400009)) ;
#9963 = CARTESIAN_POINT('',(58.7276880157606,67.9830586252741,69.2224337400009)) ;
#9964 = CARTESIAN_POINT('Origin',(58.7276880157606,67.0830586252741,69.2224337400009)) ;
#9965 = CARTESIAN_POINT('Origin',(58.7276880157606,68.5830586252741,69.2224337400009)) ;
#9966 = CARTESIAN_POINT('Origin',(40.5810116473826,66.5830586252741,69.2224337400009)) ;
#9967 = CARTESIAN_POINT('',(40.5810116473826,67.9830586252741,69.2224337400009)) ;
#9968 = CARTESIAN_POINT('Origin',(40.5810116473826,68.5830586252741,69.2224337400009)) ;
#9969 = CARTESIAN_POINT('',(40.1013291642416,67.8983170467897,69.2224337400009)) ;
#9970 = CARTESIAN_POINT('Origin',(40.5810116473826,66.5830586252741,69.2224337400009)) ;
#9971 = CARTESIAN_POINT('Origin',(39.8957509571812,68.4619992274392,69.2224337400009)) ;
#9972 = CARTESIAN_POINT('Origin',(31.3743643841387,67.4830586252741,69.2224337400009)) ;
#9973 = CARTESIAN_POINT('',(32.2652032814005,65.0404358424594,69.2224337400009)) ;
#9974 = CARTESIAN_POINT('',(31.8540468672797,66.1678002037585,69.2224337400009)) ;
#9975 = CARTESIAN_POINT('Origin',(32.0596250743401,65.604118023109,69.2224337400009)) ;
#9976 = CARTESIAN_POINT('Origin',(32.0596250743401,65.604118023109,69.2224337400009)) ;
#9977 = CARTESIAN_POINT('',(31.3743643841387,66.0830586252741,69.2224337400009)) ;
#9978 = CARTESIAN_POINT('Origin',(31.3743643841387,67.4830586252741,69.2224337400009)) ;
#9979 = CARTESIAN_POINT('',(31.3743643841387,65.4830586252741,69.8224337400008)) ;
#9980 = CARTESIAN_POINT('Origin',(31.3743643841387,65.4830586252741,69.2224337400009)) ;
#9981 = CARTESIAN_POINT('Origin',(31.3743643841387,65.4830586252741,69.2224337400009)) ;
#9982 = CARTESIAN_POINT('Origin',(60.2276880157606,67.0830586252741,67.2224337400009)) ;
#9983 = CARTESIAN_POINT('',(60.2276880157606,67.0830586252741,66.6224337400009)) ;
#9984 = CARTESIAN_POINT('Origin',(40.5810116473826,68.5830586252741,67.2224337400009)) ;
#9985 = CARTESIAN_POINT('',(40.5810116473826,67.9830586252741,67.2224337400009)) ;
#9986 = CARTESIAN_POINT('Origin',(32.0596250743401,65.6041180231089,67.2224337400009)) ;
#9987 = CARTESIAN_POINT('',(32.2652032814005,65.0404358424594,67.2224337400009)) ;
#9988 = CARTESIAN_POINT('Origin',(30.7276880157606,65.4830586252741,67.2224337400009)) ;
#9989 = CARTESIAN_POINT('',(30.7276880157606,65.4830586252741,66.6224337400009)) ;
#9990 = CARTESIAN_POINT('Origin',(60.2276880157606,67.0830586252741,69.2224337400009)) ;
#9991 = CARTESIAN_POINT('',(60.2276880157606,67.0830586252741,69.8224337400009)) ;
#9992 = CARTESIAN_POINT('Origin',(40.5810116473826,68.5830586252741,69.2224337400009)) ;
#9993 = CARTESIAN_POINT('',(40.5810116473826,67.9830586252741,69.2224337400009)) ;
#9994 = CARTESIAN_POINT('Origin',(32.0596250743401,65.6041180231089,69.2224337400009)) ;
#9995 = CARTESIAN_POINT('',(32.2652032814005,65.0404358424594,69.2224337400009)) ;
#9996 = CARTESIAN_POINT('Origin',(30.7276880157606,65.4830586252741,69.2224337400009)) ;
#9997 = CARTESIAN_POINT('',(30.7276880157606,65.4830586252741,69.8224337400009)) ;
#9998 = CARTESIAN_POINT('',(0.,0.,0.)) ;
#9999 = CARTESIAN_POINT('Origin',(24.4776880157598,67.0830586252741,103.472433740002)) ;
#10000 = CARTESIAN_POINT('',(24.4776880157598,67.9830586252741,103.472433740002)) ;
#10001 = CARTESIAN_POINT('Origin',(24.4776880157598,68.5830586252741,103.472433740002)) ;
#10002 = CARTESIAN_POINT('',(24.4776880157598,67.0830586252741,104.372433740002)) ;
#10003 = CARTESIAN_POINT('Origin',(24.4776880157598,67.0830586252741,103.472433740002)) ;
#10004 = CARTESIAN_POINT('',(25.0776880157598,67.0830586252741,104.972433740002)) ;
#10005 = CARTESIAN_POINT('Origin',(24.4776880157598,67.0830586252741,104.972433740002)) ;
#10006 = CARTESIAN_POINT('Origin',(24.4776880157598,67.0830586252741,104.972433740002)) ;
#10007 = CARTESIAN_POINT('Origin',(24.4776880157599,66.5830586252741,85.3257573716235)) ;
#10008 = CARTESIAN_POINT('',(24.4776880157599,67.8983170467897,84.8460748884825)) ;
#10009 = CARTESIAN_POINT('Origin',(24.4776880157599,68.4619992274392,84.6404966814221)) ;
#10010 = CARTESIAN_POINT('',(24.4776880157598,67.9830586252741,85.3257573716235)) ;
#10011 = CARTESIAN_POINT('Origin',(24.4776880157599,66.5830586252741,85.3257573716235)) ;
#10012 = CARTESIAN_POINT('Origin',(24.4776880157599,68.5830586252741,85.3257573716235)) ;
#10013 = CARTESIAN_POINT('Origin',(24.4776880157599,67.4830586252741,76.1191101083796)) ;
#10014 = CARTESIAN_POINT('',(25.0776880157599,65.4830586252741,76.1191101083796)) ;
#10015 = CARTESIAN_POINT('',(24.4776880157599,66.0830586252741,76.1191101083796)) ;
#10016 = CARTESIAN_POINT('Origin',(24.4776880157599,65.4830586252741,76.1191101083796)) ;
#10017 = CARTESIAN_POINT('Origin',(24.4776880157599,65.4830586252741,76.1191101083796)) ;
#10018 = CARTESIAN_POINT('',(24.4776880157599,66.1678002037585,76.5987925915206)) ;
#10019 = CARTESIAN_POINT('Origin',(24.4776880157599,67.4830586252741,76.1191101083796)) ;
#10020 = CARTESIAN_POINT('',(24.4776880157599,65.0404358424594,77.0099490056414)) ;
#10021 = CARTESIAN_POINT('Origin',(24.4776880157599,65.604118023109,76.804370798581)) ;
#10022 = CARTESIAN_POINT('Origin',(24.4776880157599,65.604118023109,76.804370798581)) ;
#10023 = CARTESIAN_POINT('Origin',(23.4776880157599,65.4830586252741,75.4724337400015)) ;
#10024 = CARTESIAN_POINT('',(25.0776880157599,65.4830586252741,75.4724337400016)) ;
#10025 = CARTESIAN_POINT('',(23.8776880157599,65.4830586252741,75.4724337400016)) ;
#10026 = CARTESIAN_POINT('Origin',(24.4776880157599,65.4830586252741,75.4724337400016)) ;
#10027 = CARTESIAN_POINT('',(23.0776880157599,65.4830586252741,75.4724337400015)) ;
#10028 = CARTESIAN_POINT('Origin',(23.4776880157599,65.4830586252741,75.4724337400015)) ;
#10029 = CARTESIAN_POINT('',(21.8776880157599,65.4830586252741,75.4724337400015)) ;
#10030 = CARTESIAN_POINT('Origin',(22.4776880157599,65.4830586252741,75.4724337400015)) ;
#10031 = CARTESIAN_POINT('Origin',(22.4776880157599,65.4830586252741,75.4724337400015)) ;
#10032 = CARTESIAN_POINT('Origin',(24.4776880157599,65.4830586252741,75.4724337400016)) ;
#10033 = CARTESIAN_POINT('Origin',(23.4776880157598,56.5830586252741,104.972433740002)) ;
#10034 = CARTESIAN_POINT('',(25.0776880157598,56.5830586252741,104.972433740002)) ;
#10035 = CARTESIAN_POINT('',(23.8776880157598,56.5830586252741,104.972433740002)) ;
#10036 = CARTESIAN_POINT('Origin',(24.4776880157598,56.5830586252741,104.972433740002)) ;
#10037 = CARTESIAN_POINT('Origin',(24.4776880157598,56.5830586252741,104.972433740002)) ;
#10038 = CARTESIAN_POINT('',(23.0776880157598,56.5830586252741,104.972433740002)) ;
#10039 = CARTESIAN_POINT('Origin',(23.4776880157598,56.5830586252741,104.972433740002)) ;
#10040 = CARTESIAN_POINT('',(21.8776880157598,56.5830586252741,104.972433740002)) ;
#10041 = CARTESIAN_POINT('Origin',(22.4776880157598,56.5830586252741,104.972433740002)) ;
#10042 = CARTESIAN_POINT('Origin',(22.4776880157598,56.5830586252741,104.972433740002)) ;
#10043 = CARTESIAN_POINT('Origin',(22.4776880157598,67.0830586252741,103.472433740002)) ;
#10044 = CARTESIAN_POINT('',(21.8776880157598,67.0830586252741,104.972433740002)) ;
#10045 = CARTESIAN_POINT('',(22.4776880157598,67.0830586252741,104.372433740002)) ;
#10046 = CARTESIAN_POINT('Origin',(22.4776880157598,67.0830586252741,104.972433740002)) ;
#10047 = CARTESIAN_POINT('Origin',(22.4776880157598,67.0830586252741,104.972433740002)) ;
#10048 = CARTESIAN_POINT('',(22.4776880157598,67.9830586252741,103.472433740002)) ;
#10049 = CARTESIAN_POINT('Origin',(22.4776880157598,67.0830586252741,103.472433740002)) ;
#10050 = CARTESIAN_POINT('Origin',(22.4776880157598,68.5830586252741,103.472433740002)) ;
#10051 = CARTESIAN_POINT('Origin',(22.4776880157599,66.5830586252741,85.3257573716235)) ;
#10052 = CARTESIAN_POINT('',(22.4776880157598,67.9830586252741,85.3257573716235)) ;
#10053 = CARTESIAN_POINT('Origin',(22.4776880157599,68.5830586252741,85.3257573716235)) ;
#10054 = CARTESIAN_POINT('',(22.4776880157599,67.8983170467897,84.8460748884825)) ;
#10055 = CARTESIAN_POINT('Origin',(22.4776880157599,66.5830586252741,85.3257573716235)) ;
#10056 = CARTESIAN_POINT('Origin',(22.4776880157599,68.4619992274392,84.6404966814221)) ;
#10057 = CARTESIAN_POINT('Origin',(22.4776880157599,67.4830586252741,76.1191101083796)) ;
#10058 = CARTESIAN_POINT('',(22.4776880157599,65.0404358424594,77.0099490056414)) ;
#10059 = CARTESIAN_POINT('',(22.4776880157599,66.1678002037585,76.5987925915206)) ;
#10060 = CARTESIAN_POINT('Origin',(22.4776880157599,65.604118023109,76.804370798581)) ;
#10061 = CARTESIAN_POINT('Origin',(22.4776880157599,65.604118023109,76.804370798581)) ;
#10062 = CARTESIAN_POINT('',(22.4776880157599,66.0830586252741,76.1191101083796)) ;
#10063 = CARTESIAN_POINT('Origin',(22.4776880157599,67.4830586252741,76.1191101083796)) ;
#10064 = CARTESIAN_POINT('',(21.8776880157599,65.4830586252741,76.1191101083796)) ;
#10065 = CARTESIAN_POINT('Origin',(22.4776880157599,65.4830586252741,76.1191101083796)) ;
#10066 = CARTESIAN_POINT('Origin',(22.4776880157599,65.4830586252741,76.1191101083796)) ;
#10067 = CARTESIAN_POINT('Origin',(24.4776880157598,67.0830586252741,104.972433740002)) ;
#10068 = CARTESIAN_POINT('',(25.0776880157598,67.0830586252741,104.972433740002)) ;
#10069 = CARTESIAN_POINT('Origin',(24.4776880157599,68.5830586252741,85.3257573716235)) ;
#10070 = CARTESIAN_POINT('',(24.4776880157599,67.9830586252741,85.3257573716235)) ;
#10071 = CARTESIAN_POINT('Origin',(24.4776880157599,65.6041180231089,76.804370798581)) ;
#10072 = CARTESIAN_POINT('',(24.4776880157599,65.0404358424594,77.0099490056414)) ;
#10073 = CARTESIAN_POINT('Origin',(24.4776880157599,65.4830586252741,75.4724337400016)) ;
#10074 = CARTESIAN_POINT('',(25.0776880157599,65.4830586252741,75.4724337400016)) ;
#10075 = CARTESIAN_POINT('Origin',(22.4776880157598,67.0830586252741,104.972433740002)) ;
#10076 = CARTESIAN_POINT('',(21.8776880157598,67.0830586252741,104.972433740002)) ;
#10077 = CARTESIAN_POINT('Origin',(22.4776880157599,68.5830586252741,85.3257573716235)) ;
#10078 = CARTESIAN_POINT('',(22.4776880157599,67.9830586252741,85.3257573716235)) ;
#10079 = CARTESIAN_POINT('Origin',(22.4776880157599,65.6041180231089,76.804370798581)) ;
#10080 = CARTESIAN_POINT('',(22.4776880157599,65.0404358424594,77.0099490056414)) ;
#10081 = CARTESIAN_POINT('Origin',(22.4776880157599,65.4830586252741,75.4724337400015)) ;
#10082 = CARTESIAN_POINT('',(21.8776880157599,65.4830586252741,75.4724337400015)) ;
#10083 = CARTESIAN_POINT('',(0.,0.,0.)) ;
#10084 = CARTESIAN_POINT('Origin',(-11.7723119842408,67.0830586252741,69.2224337400006)) ;
#10085 = CARTESIAN_POINT('',(-11.7723119842408,67.9830586252741,69.2224337400007)) ;
#10086 = CARTESIAN_POINT('Origin',(-11.7723119842408,68.5830586252741,69.2224337400006)) ;
#10087 = CARTESIAN_POINT('',(-12.6723119842408,67.0830586252741,69.2224337400006)) ;
#10088 = CARTESIAN_POINT('Origin',(-11.7723119842408,67.0830586252741,69.2224337400006)) ;
#10089 = CARTESIAN_POINT('',(-13.2723119842408,67.0830586252741,69.8224337400006)) ;
#10090 = CARTESIAN_POINT('Origin',(-13.2723119842408,67.0830586252741,69.2224337400006)) ;
#10091 = CARTESIAN_POINT('Origin',(-13.2723119842408,67.0830586252741,69.2224337400006)) ;
#10092 = CARTESIAN_POINT('Origin',(6.37436438413731,66.5830586252741,69.2224337400008)) ;
#10093 = CARTESIAN_POINT('',(6.85404686727829,67.8983170467897,69.2224337400008)) ;
#10094 = CARTESIAN_POINT('Origin',(7.05962507433871,68.4619992274392,69.2224337400008)) ;
#10095 = CARTESIAN_POINT('',(6.37436438413731,67.9830586252741,69.2224337400007)) ;
#10096 = CARTESIAN_POINT('Origin',(6.37436438413731,66.5830586252741,69.2224337400008)) ;
#10097 = CARTESIAN_POINT('Origin',(6.37436438413731,68.5830586252741,69.2224337400008)) ;
#10098 = CARTESIAN_POINT('Origin',(15.5810116473812,67.4830586252741,69.2224337400008)) ;
#10099 = CARTESIAN_POINT('',(15.5810116473812,65.4830586252741,69.8224337400008)) ;
#10100 = CARTESIAN_POINT('',(15.5810116473812,66.0830586252741,69.2224337400008)) ;
#10101 = CARTESIAN_POINT('Origin',(15.5810116473812,65.4830586252741,69.2224337400008)) ;
#10102 = CARTESIAN_POINT('Origin',(15.5810116473812,65.4830586252741,69.2224337400008)) ;
#10103 = CARTESIAN_POINT('',(15.1013291642402,66.1678002037585,69.2224337400008)) ;
#10104 = CARTESIAN_POINT('Origin',(15.5810116473812,67.4830586252741,69.2224337400008)) ;
#10105 = CARTESIAN_POINT('',(14.6901727501194,65.0404358424594,69.2224337400008)) ;
#10106 = CARTESIAN_POINT('Origin',(14.8957509571798,65.604118023109,69.2224337400008)) ;
#10107 = CARTESIAN_POINT('Origin',(14.8957509571798,65.604118023109,69.2224337400008)) ;
#10108 = CARTESIAN_POINT('Origin',(16.2276880157593,65.4830586252741,68.2224337400008)) ;
#10109 = CARTESIAN_POINT('',(16.2276880157592,65.4830586252741,69.8224337400008)) ;
#10110 = CARTESIAN_POINT('',(16.2276880157593,65.4830586252741,68.6224337400008)) ;
#10111 = CARTESIAN_POINT('Origin',(16.2276880157593,65.4830586252741,69.2224337400008)) ;
#10112 = CARTESIAN_POINT('',(16.2276880157593,65.4830586252741,67.8224337400008)) ;
#10113 = CARTESIAN_POINT('Origin',(16.2276880157593,65.4830586252741,68.2224337400008)) ;
#10114 = CARTESIAN_POINT('',(16.2276880157593,65.4830586252741,66.6224337400008)) ;
#10115 = CARTESIAN_POINT('Origin',(16.2276880157593,65.4830586252741,67.2224337400008)) ;
#10116 = CARTESIAN_POINT('Origin',(16.2276880157593,65.4830586252741,67.2224337400008)) ;
#10117 = CARTESIAN_POINT('Origin',(16.2276880157593,65.4830586252741,69.2224337400008)) ;
#10118 = CARTESIAN_POINT('Origin',(-13.2723119842407,56.5830586252741,68.2224337400006)) ;
#10119 = CARTESIAN_POINT('',(-13.2723119842408,56.5830586252741,69.8224337400006)) ;
#10120 = CARTESIAN_POINT('',(-13.2723119842407,56.5830586252741,68.6224337400006)) ;
#10121 = CARTESIAN_POINT('Origin',(-13.2723119842408,56.5830586252741,69.2224337400006)) ;
#10122 = CARTESIAN_POINT('Origin',(-13.2723119842408,56.5830586252741,69.2224337400006)) ;
#10123 = CARTESIAN_POINT('',(-13.2723119842407,56.5830586252741,67.8224337400006)) ;
#10124 = CARTESIAN_POINT('Origin',(-13.2723119842407,56.5830586252741,68.2224337400006)) ;
#10125 = CARTESIAN_POINT('',(-13.2723119842407,56.5830586252741,66.6224337400006)) ;
#10126 = CARTESIAN_POINT('Origin',(-13.2723119842407,56.5830586252741,67.2224337400006)) ;
#10127 = CARTESIAN_POINT('Origin',(-13.2723119842407,56.5830586252741,67.2224337400006)) ;
#10128 = CARTESIAN_POINT('Origin',(-11.7723119842407,67.0830586252741,67.2224337400006)) ;
#10129 = CARTESIAN_POINT('',(-13.2723119842407,67.0830586252741,66.6224337400006)) ;
#10130 = CARTESIAN_POINT('',(-12.6723119842407,67.0830586252741,67.2224337400006)) ;
#10131 = CARTESIAN_POINT('Origin',(-13.2723119842407,67.0830586252741,67.2224337400006)) ;
#10132 = CARTESIAN_POINT('Origin',(-13.2723119842407,67.0830586252741,67.2224337400006)) ;
#10133 = CARTESIAN_POINT('',(-11.7723119842407,67.9830586252741,67.2224337400007)) ;
#10134 = CARTESIAN_POINT('Origin',(-11.7723119842407,67.0830586252741,67.2224337400006)) ;
#10135 = CARTESIAN_POINT('Origin',(-11.7723119842407,68.5830586252741,67.2224337400006)) ;
#10136 = CARTESIAN_POINT('Origin',(6.37436438413732,66.5830586252741,67.2224337400008)) ;
#10137 = CARTESIAN_POINT('',(6.37436438413732,67.9830586252741,67.2224337400007)) ;
#10138 = CARTESIAN_POINT('Origin',(6.37436438413732,68.5830586252741,67.2224337400008)) ;
#10139 = CARTESIAN_POINT('',(6.8540468672783,67.8983170467897,67.2224337400008)) ;
#10140 = CARTESIAN_POINT('Origin',(6.37436438413732,66.5830586252741,67.2224337400008)) ;
#10141 = CARTESIAN_POINT('Origin',(7.05962507433873,68.4619992274392,67.2224337400008)) ;
#10142 = CARTESIAN_POINT('Origin',(15.5810116473812,67.4830586252741,67.2224337400008)) ;
#10143 = CARTESIAN_POINT('',(14.6901727501194,65.0404358424594,67.2224337400008)) ;
#10144 = CARTESIAN_POINT('',(15.1013291642402,66.1678002037585,67.2224337400008)) ;
#10145 = CARTESIAN_POINT('Origin',(14.8957509571798,65.604118023109,67.2224337400008)) ;
#10146 = CARTESIAN_POINT('Origin',(14.8957509571798,65.604118023109,67.2224337400008)) ;
#10147 = CARTESIAN_POINT('',(15.5810116473812,66.0830586252741,67.2224337400008)) ;
#10148 = CARTESIAN_POINT('Origin',(15.5810116473812,67.4830586252741,67.2224337400008)) ;
#10149 = CARTESIAN_POINT('',(15.5810116473812,65.4830586252741,66.6224337400008)) ;
#10150 = CARTESIAN_POINT('Origin',(15.5810116473812,65.4830586252741,67.2224337400008)) ;
#10151 = CARTESIAN_POINT('Origin',(15.5810116473812,65.4830586252741,67.2224337400008)) ;
#10152 = CARTESIAN_POINT('Origin',(-13.2723119842408,67.0830586252741,69.2224337400006)) ;
#10153 = CARTESIAN_POINT('',(-13.2723119842408,67.0830586252741,69.8224337400006)) ;
#10154 = CARTESIAN_POINT('Origin',(6.37436438413731,68.5830586252741,69.2224337400008)) ;
#10155 = CARTESIAN_POINT('',(6.37436438413731,67.9830586252741,69.2224337400008)) ;
#10156 = CARTESIAN_POINT('Origin',(14.8957509571798,65.6041180231089,69.2224337400008)) ;
#10157 = CARTESIAN_POINT('',(14.6901727501194,65.0404358424594,69.2224337400008)) ;
#10158 = CARTESIAN_POINT('Origin',(16.2276880157593,65.4830586252741,69.2224337400008)) ;
#10159 = CARTESIAN_POINT('',(16.2276880157593,65.4830586252741,69.8224337400008)) ;
#10160 = CARTESIAN_POINT('Origin',(-13.2723119842407,67.0830586252741,67.2224337400006)) ;
#10161 = CARTESIAN_POINT('',(-13.2723119842407,67.0830586252741,66.6224337400006)) ;
#10162 = CARTESIAN_POINT('Origin',(6.37436438413732,68.5830586252741,67.2224337400008)) ;
#10163 = CARTESIAN_POINT('',(6.37436438413732,67.9830586252741,67.2224337400008)) ;
#10164 = CARTESIAN_POINT('Origin',(14.8957509571798,65.6041180231089,67.2224337400008)) ;
#10165 = CARTESIAN_POINT('',(14.6901727501194,65.0404358424594,67.2224337400008)) ;
#10166 = CARTESIAN_POINT('Origin',(16.2276880157593,65.4830586252741,67.2224337400008)) ;
#10167 = CARTESIAN_POINT('',(16.2276880157593,65.4830586252741,66.6224337400008)) ;
#10168 = CARTESIAN_POINT('',(0.,0.,0.)) ;
#10169 = CARTESIAN_POINT('Origin',(22.4776880157603,67.0830586252741,32.9724337400001)) ;
#10170 = CARTESIAN_POINT('',(22.4776880157602,67.9830586252741,32.9724337400001)) ;
#10171 = CARTESIAN_POINT('Origin',(22.4776880157603,68.5830586252741,32.9724337400001)) ;
#10172 = CARTESIAN_POINT('',(22.4776880157603,67.0830586252741,32.0724337400002)) ;
#10173 = CARTESIAN_POINT('Origin',(22.4776880157603,67.0830586252741,32.9724337400001)) ;
#10174 = CARTESIAN_POINT('',(21.8776880157603,67.0830586252741,31.4724337400001)) ;
#10175 = CARTESIAN_POINT('Origin',(22.4776880157603,67.0830586252741,31.4724337400002)) ;
#10176 = CARTESIAN_POINT('Origin',(22.4776880157603,67.0830586252741,31.4724337400002)) ;
#10177 = CARTESIAN_POINT('Origin',(22.4776880157601,66.5830586252741,51.1191101083782)) ;
#10178 = CARTESIAN_POINT('',(22.4776880157601,67.8983170467897,51.5987925915192)) ;
#10179 = CARTESIAN_POINT('Origin',(22.4776880157601,68.4619992274392,51.8043707985796)) ;
#10180 = CARTESIAN_POINT('',(22.4776880157602,67.9830586252741,51.1191101083782)) ;
#10181 = CARTESIAN_POINT('Origin',(22.4776880157601,66.5830586252741,51.1191101083782)) ;
#10182 = CARTESIAN_POINT('Origin',(22.4776880157601,68.5830586252741,51.1191101083782)) ;
#10183 = CARTESIAN_POINT('Origin',(22.47768801576,67.4830586252741,60.3257573716221)) ;
#10184 = CARTESIAN_POINT('',(21.87768801576,65.4830586252741,60.3257573716221)) ;
#10185 = CARTESIAN_POINT('',(22.47768801576,66.0830586252741,60.3257573716221)) ;
#10186 = CARTESIAN_POINT('Origin',(22.47768801576,65.4830586252741,60.3257573716221)) ;
#10187 = CARTESIAN_POINT('Origin',(22.47768801576,65.4830586252741,60.3257573716221)) ;
#10188 = CARTESIAN_POINT('',(22.47768801576,66.1678002037585,59.8460748884811)) ;
#10189 = CARTESIAN_POINT('Origin',(22.47768801576,67.4830586252741,60.3257573716221)) ;
#10190 = CARTESIAN_POINT('',(22.47768801576,65.0404358424594,59.4349184743603)) ;
#10191 = CARTESIAN_POINT('Origin',(22.47768801576,65.604118023109,59.6404966814207)) ;
#10192 = CARTESIAN_POINT('Origin',(22.47768801576,65.604118023109,59.6404966814207)) ;
#10193 = CARTESIAN_POINT('Origin',(23.47768801576,65.4830586252741,60.9724337400002)) ;
#10194 = CARTESIAN_POINT('',(21.87768801576,65.4830586252741,60.9724337400001)) ;
#10195 = CARTESIAN_POINT('',(23.07768801576,65.4830586252741,60.9724337400002)) ;
#10196 = CARTESIAN_POINT('Origin',(22.47768801576,65.4830586252741,60.9724337400002)) ;
#10197 = CARTESIAN_POINT('',(23.87768801576,65.4830586252741,60.9724337400002)) ;
#10198 = CARTESIAN_POINT('Origin',(23.47768801576,65.4830586252741,60.9724337400002)) ;
#10199 = CARTESIAN_POINT('',(25.07768801576,65.4830586252741,60.9724337400002)) ;
#10200 = CARTESIAN_POINT('Origin',(24.47768801576,65.4830586252741,60.9724337400002)) ;
#10201 = CARTESIAN_POINT('Origin',(24.47768801576,65.4830586252741,60.9724337400002)) ;
#10202 = CARTESIAN_POINT('Origin',(22.47768801576,65.4830586252741,60.9724337400002)) ;
#10203 = CARTESIAN_POINT('Origin',(23.4776880157603,56.5830586252741,31.4724337400002)) ;
#10204 = CARTESIAN_POINT('',(21.8776880157603,56.5830586252741,31.4724337400001)) ;
#10205 = CARTESIAN_POINT('',(23.0776880157603,56.5830586252741,31.4724337400002)) ;
#10206 = CARTESIAN_POINT('Origin',(22.4776880157603,56.5830586252741,31.4724337400002)) ;
#10207 = CARTESIAN_POINT('Origin',(22.4776880157603,56.5830586252741,31.4724337400002)) ;
#10208 = CARTESIAN_POINT('',(23.8776880157603,56.5830586252741,31.4724337400002)) ;
#10209 = CARTESIAN_POINT('Origin',(23.4776880157603,56.5830586252741,31.4724337400002)) ;
#10210 = CARTESIAN_POINT('',(25.0776880157603,56.5830586252741,31.4724337400002)) ;
#10211 = CARTESIAN_POINT('Origin',(24.4776880157603,56.5830586252741,31.4724337400002)) ;
#10212 = CARTESIAN_POINT('Origin',(24.4776880157603,56.5830586252741,31.4724337400002)) ;
#10213 = CARTESIAN_POINT('Origin',(24.4776880157603,67.0830586252741,32.9724337400002)) ;
#10214 = CARTESIAN_POINT('',(25.0776880157603,67.0830586252741,31.4724337400002)) ;
#10215 = CARTESIAN_POINT('',(24.4776880157603,67.0830586252741,32.0724337400002)) ;
#10216 = CARTESIAN_POINT('Origin',(24.4776880157603,67.0830586252741,31.4724337400002)) ;
#10217 = CARTESIAN_POINT('Origin',(24.4776880157603,67.0830586252741,31.4724337400002)) ;
#10218 = CARTESIAN_POINT('',(24.4776880157602,67.9830586252741,32.9724337400002)) ;
#10219 = CARTESIAN_POINT('Origin',(24.4776880157603,67.0830586252741,32.9724337400002)) ;
#10220 = CARTESIAN_POINT('Origin',(24.4776880157603,68.5830586252741,32.9724337400002)) ;
#10221 = CARTESIAN_POINT('Origin',(24.4776880157601,66.5830586252741,51.1191101083782)) ;
#10222 = CARTESIAN_POINT('',(24.4776880157602,67.9830586252741,51.1191101083782)) ;
#10223 = CARTESIAN_POINT('Origin',(24.4776880157601,68.5830586252741,51.1191101083782)) ;
#10224 = CARTESIAN_POINT('',(24.4776880157601,67.8983170467897,51.5987925915192)) ;
#10225 = CARTESIAN_POINT('Origin',(24.4776880157601,66.5830586252741,51.1191101083782)) ;
#10226 = CARTESIAN_POINT('Origin',(24.4776880157601,68.4619992274392,51.8043707985796)) ;
#10227 = CARTESIAN_POINT('Origin',(24.47768801576,67.4830586252741,60.3257573716221)) ;
#10228 = CARTESIAN_POINT('',(24.47768801576,65.0404358424594,59.4349184743603)) ;
#10229 = CARTESIAN_POINT('',(24.47768801576,66.1678002037585,59.8460748884811)) ;
#10230 = CARTESIAN_POINT('Origin',(24.47768801576,65.604118023109,59.6404966814207)) ;
#10231 = CARTESIAN_POINT('Origin',(24.47768801576,65.604118023109,59.6404966814207)) ;
#10232 = CARTESIAN_POINT('',(24.47768801576,66.0830586252741,60.3257573716221)) ;
#10233 = CARTESIAN_POINT('Origin',(24.47768801576,67.4830586252741,60.3257573716221)) ;
#10234 = CARTESIAN_POINT('',(25.07768801576,65.4830586252741,60.3257573716221)) ;
#10235 = CARTESIAN_POINT('Origin',(24.47768801576,65.4830586252741,60.3257573716221)) ;
#10236 = CARTESIAN_POINT('Origin',(24.47768801576,65.4830586252741,60.3257573716221)) ;
#10237 = CARTESIAN_POINT('Origin',(22.4776880157603,67.0830586252741,31.4724337400002)) ;
#10238 = CARTESIAN_POINT('',(21.8776880157603,67.0830586252741,31.4724337400002)) ;
#10239 = CARTESIAN_POINT('Origin',(22.4776880157601,68.5830586252741,51.1191101083782)) ;
#10240 = CARTESIAN_POINT('',(22.4776880157601,67.9830586252741,51.1191101083782)) ;
#10241 = CARTESIAN_POINT('Origin',(22.47768801576,65.6041180231089,59.6404966814207)) ;
#10242 = CARTESIAN_POINT('',(22.47768801576,65.0404358424594,59.4349184743603)) ;
#10243 = CARTESIAN_POINT('Origin',(22.47768801576,65.4830586252741,60.9724337400002)) ;
#10244 = CARTESIAN_POINT('',(21.87768801576,65.4830586252741,60.9724337400002)) ;
#10245 = CARTESIAN_POINT('Origin',(24.4776880157603,67.0830586252741,31.4724337400002)) ;
#10246 = CARTESIAN_POINT('',(25.0776880157603,67.0830586252741,31.4724337400002)) ;
#10247 = CARTESIAN_POINT('Origin',(24.4776880157601,68.5830586252741,51.1191101083782)) ;
#10248 = CARTESIAN_POINT('',(24.4776880157601,67.9830586252741,51.1191101083782)) ;
#10249 = CARTESIAN_POINT('Origin',(24.47768801576,65.6041180231089,59.6404966814207)) ;
#10250 = CARTESIAN_POINT('',(24.47768801576,65.0404358424594,59.4349184743603)) ;
#10251 = CARTESIAN_POINT('Origin',(24.47768801576,65.4830586252741,60.9724337400002)) ;
#10252 = CARTESIAN_POINT('',(25.07768801576,65.4830586252741,60.9724337400002)) ;
#10253 = CARTESIAN_POINT('',(0.,0.,0.)) ;
#10254 = CARTESIAN_POINT('',(0.,0.,0.)) ;
#10255 = CARTESIAN_POINT('',(0.,0.,0.)) ;
#10256 = CARTESIAN_POINT('',(0.,0.,0.)) ;
#10257 = CARTESIAN_POINT('',(0.,0.,0.)) ;
#10258 = CARTESIAN_POINT('',(0.,0.,0.)) ;
#10259 = CARTESIAN_POINT('',(0.,0.,0.)) ;
#10260 = CARTESIAN_POINT('',(0.,0.,0.)) ;
#10261 = UNCERTAINTY_MEASURE_WITH_UNIT(LENGTH_MEASURE(0.001),#10335,
'DISTANCE_ACCURACY_VALUE',
'Maximum model space distance between geometric entities at asserted c
onnectivities') ;
#10262 = UNCERTAINTY_MEASURE_WITH_UNIT(LENGTH_MEASURE(0.001),#10335,
'DISTANCE_ACCURACY_VALUE',
'Maximum model space distance between geometric entities at asserted c
onnectivities') ;
#10263 = UNCERTAINTY_MEASURE_WITH_UNIT(LENGTH_MEASURE(0.001),#10335,
'DISTANCE_ACCURACY_VALUE',
'Maximum model space distance between geometric entities at asserted c
onnectivities') ;
#10264 = UNCERTAINTY_MEASURE_WITH_UNIT(LENGTH_MEASURE(0.001),#10335,
'DISTANCE_ACCURACY_VALUE',
'Maximum model space distance between geometric entities at asserted c
onnectivities') ;
#10265 = UNCERTAINTY_MEASURE_WITH_UNIT(LENGTH_MEASURE(0.001),#10335,
'DISTANCE_ACCURACY_VALUE',
'Maximum model space distance between geometric entities at asserted c
onnectivities') ;
#10266 = UNCERTAINTY_MEASURE_WITH_UNIT(LENGTH_MEASURE(0.001),#10335,
'DISTANCE_ACCURACY_VALUE',
'Maximum model space distance between geometric entities at asserted c
onnectivities') ;
#10267 = UNCERTAINTY_MEASURE_WITH_UNIT(LENGTH_MEASURE(0.001),#10335,
'DISTANCE_ACCURACY_VALUE',
'Maximum model space distance between geometric entities at asserted c
onnectivities') ;
#10268 = UNCERTAINTY_MEASURE_WITH_UNIT(LENGTH_MEASURE(0.001),#10335,
'DISTANCE_ACCURACY_VALUE',
'Maximum model space distance between geometric entities at asserted c
onnectivities') ;
#10269 = UNCERTAINTY_MEASURE_WITH_UNIT(LENGTH_MEASURE(0.001),#10335,
'DISTANCE_ACCURACY_VALUE',
'Maximum model space distance between geometric entities at asserted c
onnectivities') ;
#10270 = UNCERTAINTY_MEASURE_WITH_UNIT(LENGTH_MEASURE(0.001),#10335,
'DISTANCE_ACCURACY_VALUE',
'Maximum model space distance between geometric entities at asserted c
onnectivities') ;
#10271 = UNCERTAINTY_MEASURE_WITH_UNIT(LENGTH_MEASURE(0.001),#10335,
'DISTANCE_ACCURACY_VALUE',
'Maximum model space distance between geometric entities at asserted c
onnectivities') ;
#10272 = UNCERTAINTY_MEASURE_WITH_UNIT(LENGTH_MEASURE(0.001),#10335,
'DISTANCE_ACCURACY_VALUE',
'Maximum model space distance between geometric entities at asserted c
onnectivities') ;
#10273 = UNCERTAINTY_MEASURE_WITH_UNIT(LENGTH_MEASURE(0.001),#10335,
'DISTANCE_ACCURACY_VALUE',
'Maximum model space distance between geometric entities at asserted c
onnectivities') ;
#10274 = UNCERTAINTY_MEASURE_WITH_UNIT(LENGTH_MEASURE(0.001),#10335,
'DISTANCE_ACCURACY_VALUE',
'Maximum model space distance between geometric entities at asserted c
onnectivities') ;
#10275 = UNCERTAINTY_MEASURE_WITH_UNIT(LENGTH_MEASURE(0.001),#10335,
'DISTANCE_ACCURACY_VALUE',
'Maximum model space distance between geometric entities at asserted c
onnectivities') ;
#10276 = UNCERTAINTY_MEASURE_WITH_UNIT(LENGTH_MEASURE(0.001),#10335,
'DISTANCE_ACCURACY_VALUE',
'Maximum model space distance between geometric entities at asserted c
onnectivities') ;
#10277 = UNCERTAINTY_MEASURE_WITH_UNIT(LENGTH_MEASURE(0.001),#10335,
'DISTANCE_ACCURACY_VALUE',
'Maximum model space distance between geometric entities at asserted c
onnectivities') ;
#10278 = UNCERTAINTY_MEASURE_WITH_UNIT(LENGTH_MEASURE(0.001),#10335,
'DISTANCE_ACCURACY_VALUE',
'Maximum model space distance between geometric entities at asserted c
onnectivities') ;
#10279 = UNCERTAINTY_MEASURE_WITH_UNIT(LENGTH_MEASURE(0.001),#10335,
'DISTANCE_ACCURACY_VALUE',
'Maximum model space distance between geometric entities at asserted c
onnectivities') ;
#10280 = UNCERTAINTY_MEASURE_WITH_UNIT(LENGTH_MEASURE(0.001),#10335,
'DISTANCE_ACCURACY_VALUE',
'Maximum model space distance between geometric entities at asserted c
onnectivities') ;
#10281 = UNCERTAINTY_MEASURE_WITH_UNIT(LENGTH_MEASURE(0.001),#10335,
'DISTANCE_ACCURACY_VALUE',
'Maximum model space distance between geometric entities at asserted c
onnectivities') ;
#10282 = UNCERTAINTY_MEASURE_WITH_UNIT(LENGTH_MEASURE(0.001),#10335,
'DISTANCE_ACCURACY_VALUE',
'Maximum model space distance between geometric entities at asserted c
onnectivities') ;
#10283 = UNCERTAINTY_MEASURE_WITH_UNIT(LENGTH_MEASURE(0.001),#10335,
'DISTANCE_ACCURACY_VALUE',
'Maximum model space distance between geometric entities at asserted c
onnectivities') ;
#10284 = UNCERTAINTY_MEASURE_WITH_UNIT(LENGTH_MEASURE(0.001),#10335,
'DISTANCE_ACCURACY_VALUE',
'Maximum model space distance between geometric entities at asserted c
onnectivities') ;
#10285 = UNCERTAINTY_MEASURE_WITH_UNIT(LENGTH_MEASURE(0.001),#10335,
'DISTANCE_ACCURACY_VALUE',
'Maximum model space distance between geometric entities at asserted c
onnectivities') ;
#10286 = UNCERTAINTY_MEASURE_WITH_UNIT(LENGTH_MEASURE(0.001),#10335,
'DISTANCE_ACCURACY_VALUE',
'Maximum model space distance between geometric entities at asserted c
onnectivities') ;
#10287 = UNCERTAINTY_MEASURE_WITH_UNIT(LENGTH_MEASURE(0.001),#10335,
'DISTANCE_ACCURACY_VALUE',
'Maximum model space distance between geometric entities at asserted c
onnectivities') ;
#10288 = UNCERTAINTY_MEASURE_WITH_UNIT(LENGTH_MEASURE(0.001),#10335,
'DISTANCE_ACCURACY_VALUE',
'Maximum model space distance between geometric entities at asserted c
onnectivities') ;
#10289 = UNCERTAINTY_MEASURE_WITH_UNIT(LENGTH_MEASURE(0.001),#10335,
'DISTANCE_ACCURACY_VALUE',
'Maximum model space distance between geometric entities at asserted c
onnectivities') ;
#10290 = UNCERTAINTY_MEASURE_WITH_UNIT(LENGTH_MEASURE(0.001),#10335,
'DISTANCE_ACCURACY_VALUE',
'Maximum model space distance between geometric entities at asserted c
onnectivities') ;
#10291 = UNCERTAINTY_MEASURE_WITH_UNIT(LENGTH_MEASURE(0.001),#10335,
'DISTANCE_ACCURACY_VALUE',
'Maximum model space distance between geometric entities at asserted c
onnectivities') ;
#10292 = UNCERTAINTY_MEASURE_WITH_UNIT(LENGTH_MEASURE(0.001),#10335,
'DISTANCE_ACCURACY_VALUE',
'Maximum model space distance between geometric entities at asserted c
onnectivities') ;
#10293 = UNCERTAINTY_MEASURE_WITH_UNIT(LENGTH_MEASURE(0.001),#10335,
'DISTANCE_ACCURACY_VALUE',
'Maximum model space distance between geometric entities at asserted c
onnectivities') ;
#10294 = UNCERTAINTY_MEASURE_WITH_UNIT(LENGTH_MEASURE(0.001),#10335,
'DISTANCE_ACCURACY_VALUE',
'Maximum model space distance between geometric entities at asserted c
onnectivities') ;
#10295 = UNCERTAINTY_MEASURE_WITH_UNIT(LENGTH_MEASURE(0.001),#10335,
'DISTANCE_ACCURACY_VALUE',
'Maximum model space distance between geometric entities at asserted c
onnectivities') ;
#10296 = UNCERTAINTY_MEASURE_WITH_UNIT(LENGTH_MEASURE(0.001),#10335,
'DISTANCE_ACCURACY_VALUE',
'Maximum model space distance between geometric entities at asserted c
onnectivities') ;
#10297 = UNCERTAINTY_MEASURE_WITH_UNIT(LENGTH_MEASURE(0.001),#10335,
'DISTANCE_ACCURACY_VALUE',
'Maximum model space distance between geometric entities at asserted c
onnectivities') ;
#10298 = (
GEOMETRIC_REPRESENTATION_CONTEXT(3)
GLOBAL_UNCERTAINTY_ASSIGNED_CONTEXT((#10261))
GLOBAL_UNIT_ASSIGNED_CONTEXT((#10335,#10337,#10338))
REPRESENTATION_CONTEXT('','3D')
) ;
#10299 = (
GEOMETRIC_REPRESENTATION_CONTEXT(3)
GLOBAL_UNCERTAINTY_ASSIGNED_CONTEXT((#10262))
GLOBAL_UNIT_ASSIGNED_CONTEXT((#10335,#10337,#10338))
REPRESENTATION_CONTEXT('','3D')
) ;
#10300 = (
GEOMETRIC_REPRESENTATION_CONTEXT(3)
GLOBAL_UNCERTAINTY_ASSIGNED_CONTEXT((#10263))
GLOBAL_UNIT_ASSIGNED_CONTEXT((#10335,#10337,#10338))
REPRESENTATION_CONTEXT('','3D')
) ;
#10301 = (
GEOMETRIC_REPRESENTATION_CONTEXT(3)
GLOBAL_UNCERTAINTY_ASSIGNED_CONTEXT((#10264))
GLOBAL_UNIT_ASSIGNED_CONTEXT((#10335,#10337,#10338))
REPRESENTATION_CONTEXT('','3D')
) ;
#10302 = (
GEOMETRIC_REPRESENTATION_CONTEXT(3)
GLOBAL_UNCERTAINTY_ASSIGNED_CONTEXT((#10265))
GLOBAL_UNIT_ASSIGNED_CONTEXT((#10335,#10337,#10338))
REPRESENTATION_CONTEXT('','3D')
) ;
#10303 = (
GEOMETRIC_REPRESENTATION_CONTEXT(3)
GLOBAL_UNCERTAINTY_ASSIGNED_CONTEXT((#10266))
GLOBAL_UNIT_ASSIGNED_CONTEXT((#10335,#10337,#10338))
REPRESENTATION_CONTEXT('','3D')
) ;
#10304 = (
GEOMETRIC_REPRESENTATION_CONTEXT(3)
GLOBAL_UNCERTAINTY_ASSIGNED_CONTEXT((#10267))
GLOBAL_UNIT_ASSIGNED_CONTEXT((#10335,#10337,#10338))
REPRESENTATION_CONTEXT('','3D')
) ;
#10305 = (
GEOMETRIC_REPRESENTATION_CONTEXT(3)
GLOBAL_UNCERTAINTY_ASSIGNED_CONTEXT((#10268))
GLOBAL_UNIT_ASSIGNED_CONTEXT((#10335,#10337,#10338))
REPRESENTATION_CONTEXT('','3D')
) ;
#10306 = (
GEOMETRIC_REPRESENTATION_CONTEXT(3)
GLOBAL_UNCERTAINTY_ASSIGNED_CONTEXT((#10269))
GLOBAL_UNIT_ASSIGNED_CONTEXT((#10335,#10337,#10338))
REPRESENTATION_CONTEXT('','3D')
) ;
#10307 = (
GEOMETRIC_REPRESENTATION_CONTEXT(3)
GLOBAL_UNCERTAINTY_ASSIGNED_CONTEXT((#10270))
GLOBAL_UNIT_ASSIGNED_CONTEXT((#10335,#10337,#10338))
REPRESENTATION_CONTEXT('','3D')
) ;
#10308 = (
GEOMETRIC_REPRESENTATION_CONTEXT(3)
GLOBAL_UNCERTAINTY_ASSIGNED_CONTEXT((#10271))
GLOBAL_UNIT_ASSIGNED_CONTEXT((#10335,#10337,#10338))
REPRESENTATION_CONTEXT('','3D')
) ;
#10309 = (
GEOMETRIC_REPRESENTATION_CONTEXT(3)
GLOBAL_UNCERTAINTY_ASSIGNED_CONTEXT((#10272))
GLOBAL_UNIT_ASSIGNED_CONTEXT((#10335,#10337,#10338))
REPRESENTATION_CONTEXT('','3D')
) ;
#10310 = (
GEOMETRIC_REPRESENTATION_CONTEXT(3)
GLOBAL_UNCERTAINTY_ASSIGNED_CONTEXT((#10273))
GLOBAL_UNIT_ASSIGNED_CONTEXT((#10335,#10337,#10338))
REPRESENTATION_CONTEXT('','3D')
) ;
#10311 = (
GEOMETRIC_REPRESENTATION_CONTEXT(3)
GLOBAL_UNCERTAINTY_ASSIGNED_CONTEXT((#10274))
GLOBAL_UNIT_ASSIGNED_CONTEXT((#10335,#10337,#10338))
REPRESENTATION_CONTEXT('','3D')
) ;
#10312 = (
GEOMETRIC_REPRESENTATION_CONTEXT(3)
GLOBAL_UNCERTAINTY_ASSIGNED_CONTEXT((#10275))
GLOBAL_UNIT_ASSIGNED_CONTEXT((#10335,#10337,#10338))
REPRESENTATION_CONTEXT('','3D')
) ;
#10313 = (
GEOMETRIC_REPRESENTATION_CONTEXT(3)
GLOBAL_UNCERTAINTY_ASSIGNED_CONTEXT((#10276))
GLOBAL_UNIT_ASSIGNED_CONTEXT((#10335,#10337,#10338))
REPRESENTATION_CONTEXT('','3D')
) ;
#10314 = (
GEOMETRIC_REPRESENTATION_CONTEXT(3)
GLOBAL_UNCERTAINTY_ASSIGNED_CONTEXT((#10277))
GLOBAL_UNIT_ASSIGNED_CONTEXT((#10335,#10337,#10338))
REPRESENTATION_CONTEXT('','3D')
) ;
#10315 = (
GEOMETRIC_REPRESENTATION_CONTEXT(3)
GLOBAL_UNCERTAINTY_ASSIGNED_CONTEXT((#10278))
GLOBAL_UNIT_ASSIGNED_CONTEXT((#10335,#10337,#10338))
REPRESENTATION_CONTEXT('','3D')
) ;
#10316 = (
GEOMETRIC_REPRESENTATION_CONTEXT(3)
GLOBAL_UNCERTAINTY_ASSIGNED_CONTEXT((#10279))
GLOBAL_UNIT_ASSIGNED_CONTEXT((#10335,#10337,#10338))
REPRESENTATION_CONTEXT('','3D')
) ;
#10317 = (
GEOMETRIC_REPRESENTATION_CONTEXT(3)
GLOBAL_UNCERTAINTY_ASSIGNED_CONTEXT((#10280))
GLOBAL_UNIT_ASSIGNED_CONTEXT((#10335,#10337,#10338))
REPRESENTATION_CONTEXT('','3D')
) ;
#10318 = (
GEOMETRIC_REPRESENTATION_CONTEXT(3)
GLOBAL_UNCERTAINTY_ASSIGNED_CONTEXT((#10281))
GLOBAL_UNIT_ASSIGNED_CONTEXT((#10335,#10337,#10338))
REPRESENTATION_CONTEXT('','3D')
) ;
#10319 = (
GEOMETRIC_REPRESENTATION_CONTEXT(3)
GLOBAL_UNCERTAINTY_ASSIGNED_CONTEXT((#10282))
GLOBAL_UNIT_ASSIGNED_CONTEXT((#10335,#10337,#10338))
REPRESENTATION_CONTEXT('','3D')
) ;
#10320 = (
GEOMETRIC_REPRESENTATION_CONTEXT(3)
GLOBAL_UNCERTAINTY_ASSIGNED_CONTEXT((#10283))
GLOBAL_UNIT_ASSIGNED_CONTEXT((#10335,#10337,#10338))
REPRESENTATION_CONTEXT('','3D')
) ;
#10321 = (
GEOMETRIC_REPRESENTATION_CONTEXT(3)
GLOBAL_UNCERTAINTY_ASSIGNED_CONTEXT((#10284))
GLOBAL_UNIT_ASSIGNED_CONTEXT((#10335,#10337,#10338))
REPRESENTATION_CONTEXT('','3D')
) ;
#10322 = (
GEOMETRIC_REPRESENTATION_CONTEXT(3)
GLOBAL_UNCERTAINTY_ASSIGNED_CONTEXT((#10285))
GLOBAL_UNIT_ASSIGNED_CONTEXT((#10335,#10337,#10338))
REPRESENTATION_CONTEXT('','3D')
) ;
#10323 = (
GEOMETRIC_REPRESENTATION_CONTEXT(3)
GLOBAL_UNCERTAINTY_ASSIGNED_CONTEXT((#10286))
GLOBAL_UNIT_ASSIGNED_CONTEXT((#10335,#10337,#10338))
REPRESENTATION_CONTEXT('','3D')
) ;
#10324 = (
GEOMETRIC_REPRESENTATION_CONTEXT(3)
GLOBAL_UNCERTAINTY_ASSIGNED_CONTEXT((#10287))
GLOBAL_UNIT_ASSIGNED_CONTEXT((#10335,#10337,#10338))
REPRESENTATION_CONTEXT('','3D')
) ;
#10325 = (
GEOMETRIC_REPRESENTATION_CONTEXT(3)
GLOBAL_UNCERTAINTY_ASSIGNED_CONTEXT((#10288))
GLOBAL_UNIT_ASSIGNED_CONTEXT((#10335,#10337,#10338))
REPRESENTATION_CONTEXT('','3D')
) ;
#10326 = (
GEOMETRIC_REPRESENTATION_CONTEXT(3)
GLOBAL_UNCERTAINTY_ASSIGNED_CONTEXT((#10289))
GLOBAL_UNIT_ASSIGNED_CONTEXT((#10335,#10337,#10338))
REPRESENTATION_CONTEXT('','3D')
) ;
#10327 = (
GEOMETRIC_REPRESENTATION_CONTEXT(3)
GLOBAL_UNCERTAINTY_ASSIGNED_CONTEXT((#10290))
GLOBAL_UNIT_ASSIGNED_CONTEXT((#10335,#10337,#10338))
REPRESENTATION_CONTEXT('','3D')
) ;
#10328 = (
GEOMETRIC_REPRESENTATION_CONTEXT(3)
GLOBAL_UNCERTAINTY_ASSIGNED_CONTEXT((#10291))
GLOBAL_UNIT_ASSIGNED_CONTEXT((#10335,#10337,#10338))
REPRESENTATION_CONTEXT('','3D')
) ;
#10329 = (
GEOMETRIC_REPRESENTATION_CONTEXT(3)
GLOBAL_UNCERTAINTY_ASSIGNED_CONTEXT((#10292))
GLOBAL_UNIT_ASSIGNED_CONTEXT((#10335,#10337,#10338))
REPRESENTATION_CONTEXT('','3D')
) ;
#10330 = (
GEOMETRIC_REPRESENTATION_CONTEXT(3)
GLOBAL_UNCERTAINTY_ASSIGNED_CONTEXT((#10293))
GLOBAL_UNIT_ASSIGNED_CONTEXT((#10335,#10337,#10338))
REPRESENTATION_CONTEXT('','3D')
) ;
#10331 = (
GEOMETRIC_REPRESENTATION_CONTEXT(3)
GLOBAL_UNCERTAINTY_ASSIGNED_CONTEXT((#10294))
GLOBAL_UNIT_ASSIGNED_CONTEXT((#10335,#10337,#10338))
REPRESENTATION_CONTEXT('','3D')
) ;
#10332 = (
GEOMETRIC_REPRESENTATION_CONTEXT(3)
GLOBAL_UNCERTAINTY_ASSIGNED_CONTEXT((#10295))
GLOBAL_UNIT_ASSIGNED_CONTEXT((#10335,#10337,#10338))
REPRESENTATION_CONTEXT('','3D')
) ;
#10333 = (
GEOMETRIC_REPRESENTATION_CONTEXT(3)
GLOBAL_UNCERTAINTY_ASSIGNED_CONTEXT((#10296))
GLOBAL_UNIT_ASSIGNED_CONTEXT((#10335,#10337,#10338))
REPRESENTATION_CONTEXT('','3D')
) ;
#10334 = (
GEOMETRIC_REPRESENTATION_CONTEXT(3)
GLOBAL_UNCERTAINTY_ASSIGNED_CONTEXT((#10297))
GLOBAL_UNIT_ASSIGNED_CONTEXT((#10335,#10337,#10338))
REPRESENTATION_CONTEXT('','3D')
) ;
#10335 = (
LENGTH_UNIT()
NAMED_UNIT(*)
SI_UNIT(.CENTI.,.METRE.)
) ;
#10336 = (
LENGTH_UNIT()
NAMED_UNIT(*)
SI_UNIT($,.METRE.)
) ;
#10337 = (
NAMED_UNIT(*)
PLANE_ANGLE_UNIT()
SI_UNIT($,.RADIAN.)
) ;
#10338 = (
NAMED_UNIT(*)
SI_UNIT($,.STERADIAN.)
SOLID_ANGLE_UNIT()
) ;
#10339 = SHAPE_DEFINITION_REPRESENTATION(#10375,#10446) ;
#10340 = SHAPE_DEFINITION_REPRESENTATION(#10376,#10447) ;
#10341 = SHAPE_DEFINITION_REPRESENTATION(#10377,#10448) ;
#10342 = SHAPE_DEFINITION_REPRESENTATION(#10378,#10449) ;
#10343 = SHAPE_DEFINITION_REPRESENTATION(#10379,#10450) ;
#10344 = SHAPE_DEFINITION_REPRESENTATION(#10380,#10451) ;
#10345 = SHAPE_DEFINITION_REPRESENTATION(#10381,#10452) ;
#10346 = SHAPE_DEFINITION_REPRESENTATION(#10382,#10453) ;
#10347 = SHAPE_DEFINITION_REPRESENTATION(#10383,#10454) ;
#10348 = SHAPE_DEFINITION_REPRESENTATION(#10384,#10455) ;
#10349 = SHAPE_DEFINITION_REPRESENTATION(#10385,#10456) ;
#10350 = SHAPE_DEFINITION_REPRESENTATION(#10386,#10457) ;
#10351 = SHAPE_DEFINITION_REPRESENTATION(#10387,#10458) ;
#10352 = SHAPE_DEFINITION_REPRESENTATION(#10388,#10459) ;
#10353 = SHAPE_DEFINITION_REPRESENTATION(#10389,#10460) ;
#10354 = SHAPE_DEFINITION_REPRESENTATION(#10390,#10461) ;
#10355 = SHAPE_DEFINITION_REPRESENTATION(#10391,#10462) ;
#10356 = SHAPE_DEFINITION_REPRESENTATION(#10392,#10463) ;
#10357 = SHAPE_DEFINITION_REPRESENTATION(#10393,#10464) ;
#10358 = SHAPE_DEFINITION_REPRESENTATION(#10394,#10465) ;
#10359 = SHAPE_DEFINITION_REPRESENTATION(#10395,#10466) ;
#10360 = SHAPE_DEFINITION_REPRESENTATION(#10396,#10467) ;
#10361 = SHAPE_DEFINITION_REPRESENTATION(#10397,#10468) ;
#10362 = SHAPE_DEFINITION_REPRESENTATION(#10398,#10469) ;
#10363 = SHAPE_DEFINITION_REPRESENTATION(#10399,#10470) ;
#10364 = SHAPE_DEFINITION_REPRESENTATION(#10400,#10471) ;
#10365 = SHAPE_DEFINITION_REPRESENTATION(#10425,#10472) ;
#10366 = SHAPE_DEFINITION_REPRESENTATION(#10426,#10473) ;
#10367 = SHAPE_DEFINITION_REPRESENTATION(#10427,#10474) ;
#10368 = SHAPE_DEFINITION_REPRESENTATION(#10428,#10475) ;
#10369 = SHAPE_DEFINITION_REPRESENTATION(#10432,#10476) ;
#10370 = SHAPE_DEFINITION_REPRESENTATION(#10433,#10477) ;
#10371 = SHAPE_DEFINITION_REPRESENTATION(#10434,#10478) ;
#10372 = SHAPE_DEFINITION_REPRESENTATION(#10435,#10479) ;
#10373 = SHAPE_DEFINITION_REPRESENTATION(#10436,#10480) ;
#10374 = SHAPE_DEFINITION_REPRESENTATION(#10437,#10481) ;
#10375 = PRODUCT_DEFINITION_SHAPE('',$,#10483) ;
#10376 = PRODUCT_DEFINITION_SHAPE('',$,#10484) ;
#10377 = PRODUCT_DEFINITION_SHAPE('',$,#10485) ;
#10378 = PRODUCT_DEFINITION_SHAPE('',$,#10486) ;
#10379 = PRODUCT_DEFINITION_SHAPE('',$,#10487) ;
#10380 = PRODUCT_DEFINITION_SHAPE('',$,#10488) ;
#10381 = PRODUCT_DEFINITION_SHAPE('',$,#10489) ;
#10382 = PRODUCT_DEFINITION_SHAPE('',$,#10490) ;
#10383 = PRODUCT_DEFINITION_SHAPE('',$,#10491) ;
#10384 = PRODUCT_DEFINITION_SHAPE('',$,#10492) ;
#10385 = PRODUCT_DEFINITION_SHAPE('',$,#10493) ;
#10386 = PRODUCT_DEFINITION_SHAPE('',$,#10494) ;
#10387 = PRODUCT_DEFINITION_SHAPE('',$,#10495) ;
#10388 = PRODUCT_DEFINITION_SHAPE('',$,#10496) ;
#10389 = PRODUCT_DEFINITION_SHAPE('',$,#10497) ;
#10390 = PRODUCT_DEFINITION_SHAPE('',$,#10498) ;
#10391 = PRODUCT_DEFINITION_SHAPE('',$,#10499) ;
#10392 = PRODUCT_DEFINITION_SHAPE('',$,#10500) ;
#10393 = PRODUCT_DEFINITION_SHAPE('',$,#10501) ;
#10394 = PRODUCT_DEFINITION_SHAPE('',$,#10502) ;
#10395 = PRODUCT_DEFINITION_SHAPE('',$,#10503) ;
#10396 = PRODUCT_DEFINITION_SHAPE('',$,#10504) ;
#10397 = PRODUCT_DEFINITION_SHAPE('',$,#10505) ;
#10398 = PRODUCT_DEFINITION_SHAPE('',$,#10506) ;
#10399 = PRODUCT_DEFINITION_SHAPE('',$,#10507) ;
#10400 = PRODUCT_DEFINITION_SHAPE('',$,#10508) ;
#10401 = PRODUCT_DEFINITION_SHAPE($,$,#297) ;
#10402 = PRODUCT_DEFINITION_SHAPE($,$,#298) ;
#10403 = PRODUCT_DEFINITION_SHAPE($,$,#299) ;
#10404 = PRODUCT_DEFINITION_SHAPE($,$,#300) ;
#10405 = PRODUCT_DEFINITION_SHAPE($,$,#301) ;
#10406 = PRODUCT_DEFINITION_SHAPE($,$,#302) ;
#10407 = PRODUCT_DEFINITION_SHAPE($,$,#303) ;
#10408 = PRODUCT_DEFINITION_SHAPE($,$,#304) ;
#10409 = PRODUCT_DEFINITION_SHAPE($,$,#305) ;
#10410 = PRODUCT_DEFINITION_SHAPE($,$,#306) ;
#10411 = PRODUCT_DEFINITION_SHAPE($,$,#307) ;
#10412 = PRODUCT_DEFINITION_SHAPE($,$,#308) ;
#10413 = PRODUCT_DEFINITION_SHAPE($,$,#309) ;
#10414 = PRODUCT_DEFINITION_SHAPE($,$,#310) ;
#10415 = PRODUCT_DEFINITION_SHAPE($,$,#311) ;
#10416 = PRODUCT_DEFINITION_SHAPE($,$,#312) ;
#10417 = PRODUCT_DEFINITION_SHAPE($,$,#313) ;
#10418 = PRODUCT_DEFINITION_SHAPE($,$,#314) ;
#10419 = PRODUCT_DEFINITION_SHAPE($,$,#315) ;
#10420 = PRODUCT_DEFINITION_SHAPE($,$,#316) ;
#10421 = PRODUCT_DEFINITION_SHAPE($,$,#317) ;
#10422 = PRODUCT_DEFINITION_SHAPE($,$,#318) ;
#10423 = PRODUCT_DEFINITION_SHAPE($,$,#319) ;
#10424 = PRODUCT_DEFINITION_SHAPE($,$,#320) ;
#10425 = PRODUCT_DEFINITION_SHAPE('',$,#10509) ;
#10426 = PRODUCT_DEFINITION_SHAPE('',$,#10510) ;
#10427 = PRODUCT_DEFINITION_SHAPE('',$,#10511) ;
#10428 = PRODUCT_DEFINITION_SHAPE('',$,#10512) ;
#10429 = PRODUCT_DEFINITION_SHAPE($,$,#321) ;
#10430 = PRODUCT_DEFINITION_SHAPE($,$,#322) ;
#10431 = PRODUCT_DEFINITION_SHAPE($,$,#323) ;
#10432 = PRODUCT_DEFINITION_SHAPE('',$,#10513) ;
#10433 = PRODUCT_DEFINITION_SHAPE('',$,#10514) ;
#10434 = PRODUCT_DEFINITION_SHAPE('',$,#10515) ;
#10435 = PRODUCT_DEFINITION_SHAPE('',$,#10516) ;
#10436 = PRODUCT_DEFINITION_SHAPE('',$,#10517) ;
#10437 = PRODUCT_DEFINITION_SHAPE('',$,#10518) ;
#10438 = PRODUCT_DEFINITION_SHAPE($,$,#324) ;
#10439 = PRODUCT_DEFINITION_SHAPE($,$,#325) ;
#10440 = PRODUCT_DEFINITION_SHAPE($,$,#326) ;
#10441 = PRODUCT_DEFINITION_SHAPE($,$,#327) ;
#10442 = PRODUCT_DEFINITION_SHAPE($,$,#328) ;
#10443 = PRODUCT_DEFINITION_SHAPE($,$,#329) ;
#10444 = PRODUCT_DEFINITION_SHAPE($,$,#330) ;
#10445 = PRODUCT_DEFINITION_SHAPE($,$,#331) ;
#10446 = SHAPE_REPRESENTATION('',(#3943,#4441,#4442,#4443),#10298) ;
#10447 = SHAPE_REPRESENTATION('',(#3944,#4061,#4062,#4063,#4064,#4065,#4066,
#4067,#4068,#4069,#4070,#4071,#4072,#4073,#4074,#4075,#4076,#4077,#4078,
#4079,#4080,#4081,#4082,#4083,#4084),#10299) ;
#10448 = SHAPE_REPRESENTATION('',(#3945),#10300) ;
#10449 = SHAPE_REPRESENTATION('',(#3958),#10301) ;
#10450 = SHAPE_REPRESENTATION('',(#3973),#10302) ;
#10451 = SHAPE_REPRESENTATION('',(#3977),#10303) ;
#10452 = SHAPE_REPRESENTATION('',(#3981),#10304) ;
#10453 = SHAPE_REPRESENTATION('',(#3985),#10305) ;
#10454 = SHAPE_REPRESENTATION('',(#3989),#10306) ;
#10455 = SHAPE_REPRESENTATION('',(#3993),#10307) ;
#10456 = SHAPE_REPRESENTATION('',(#3997),#10308) ;
#10457 = SHAPE_REPRESENTATION('',(#4001),#10309) ;
#10458 = SHAPE_REPRESENTATION('',(#4005),#10310) ;
#10459 = SHAPE_REPRESENTATION('',(#4009),#10311) ;
#10460 = SHAPE_REPRESENTATION('',(#4013),#10312) ;
#10461 = SHAPE_REPRESENTATION('',(#4017),#10313) ;
#10462 = SHAPE_REPRESENTATION('',(#4021),#10314) ;
#10463 = SHAPE_REPRESENTATION('',(#4025),#10315) ;
#10464 = SHAPE_REPRESENTATION('',(#4029),#10316) ;
#10465 = SHAPE_REPRESENTATION('',(#4033),#10317) ;
#10466 = SHAPE_REPRESENTATION('',(#4037),#10318) ;
#10467 = SHAPE_REPRESENTATION('',(#4041),#10319) ;
#10468 = SHAPE_REPRESENTATION('',(#4045),#10320) ;
#10469 = SHAPE_REPRESENTATION('',(#4049),#10321) ;
#10470 = SHAPE_REPRESENTATION('',(#4053),#10322) ;
#10471 = SHAPE_REPRESENTATION('',(#4057),#10323) ;
#10472 = SHAPE_REPRESENTATION('',(#4085,#4166,#4167,#4168),#10324) ;
#10473 = SHAPE_REPRESENTATION('',(#4086),#10325) ;
#10474 = SHAPE_REPRESENTATION('',(#4138),#10326) ;
#10475 = SHAPE_REPRESENTATION('',(#4147),#10327) ;
#10476 = SHAPE_REPRESENTATION('',(#4169,#4436,#4437,#4438,#4439,#4440),#10328) ;
#10477 = SHAPE_REPRESENTATION('',(#4170),#10329) ;
#10478 = SHAPE_REPRESENTATION('',(#4232),#10330) ;
#10479 = SHAPE_REPRESENTATION('',(#4283),#10331) ;
#10480 = SHAPE_REPRESENTATION('',(#4334),#10332) ;
#10481 = SHAPE_REPRESENTATION('',(#4385),#10333) ;
#10482 = PRODUCT_DEFINITION_CONTEXT('part definition',#10592,'design') ;
#10483 = PRODUCT_DEFINITION('MAS-638','MAS-638',#10519,
#10482) ;
#10484 = PRODUCT_DEFINITION('Guard_Assembly','Guard_Assembly',#10520,#10482) ;
#10485 = PRODUCT_DEFINITION('Guard_Mounting_Ring_1',
'Guard_Mounting_Ring_1',#10521,#10482) ;
#10486 = PRODUCT_DEFINITION('Guard_Mounting_Ring_2',
'Guard_Mounting_Ring_2',#10522,#10482) ;
#10487 = PRODUCT_DEFINITION('Guard_Ring_1','Guard_Ring_1',#10523,#10482) ;
#10488 = PRODUCT_DEFINITION('Guard_Ring_2','Guard_Ring_2',#10524,#10482) ;
#10489 = PRODUCT_DEFINITION('Guard_Ring_3','Guard_Ring_3',#10525,#10482) ;
#10490 = PRODUCT_DEFINITION('Guard_Ring_4','Guard_Ring_4',#10526,#10482) ;
#10491 = PRODUCT_DEFINITION('Guard_Ring_5','Guard_Ring_5',#10527,#10482) ;
#10492 = PRODUCT_DEFINITION('Guard_Ring_6','Guard_Ring_6',#10528,#10482) ;
#10493 = PRODUCT_DEFINITION('Guard_Ring_7','Guard_Ring_7',#10529,#10482) ;
#10494 = PRODUCT_DEFINITION('Guard_Ring_8','Guard_Ring_8',#10530,#10482) ;
#10495 = PRODUCT_DEFINITION('Guard_Ring_9','Guard_Ring_9',#10531,#10482) ;
#10496 = PRODUCT_DEFINITION('Guard_Ring_10','Guard_Ring_10',#10532,#10482) ;
#10497 = PRODUCT_DEFINITION('Guard_Ring_11','Guard_Ring_11',#10533,#10482) ;
#10498 = PRODUCT_DEFINITION('Guard_Ring_12','Guard_Ring_12',#10534,#10482) ;
#10499 = PRODUCT_DEFINITION('Guard_Ring_13','Guard_Ring_13',#10535,#10482) ;
#10500 = PRODUCT_DEFINITION('Guard_Ring_14','Guard_Ring_14',#10536,#10482) ;
#10501 = PRODUCT_DEFINITION('Guard_Ring_15','Guard_Ring_15',#10537,#10482) ;
#10502 = PRODUCT_DEFINITION('Guard_Ring_16','Guard_Ring_16',#10538,#10482) ;
#10503 = PRODUCT_DEFINITION('Guard_Ring_17','Guard_Ring_17',#10539,#10482) ;
#10504 = PRODUCT_DEFINITION('Guard_Ring_18','Guard_Ring_18',#10540,#10482) ;
#10505 = PRODUCT_DEFINITION('Guard_Ring_19','Guard_Ring_19',#10541,#10482) ;
#10506 = PRODUCT_DEFINITION('Guard_Ring_20','Guard_Ring_20',#10542,#10482) ;
#10507 = PRODUCT_DEFINITION('Guard_Ring_21','Guard_Ring_21',#10543,#10482) ;
#10508 = PRODUCT_DEFINITION('Guard_Ring_22','Guard_Ring_22',#10544,#10482) ;
#10509 = PRODUCT_DEFINITION('Fan_Assembly','Fan_Assembly',#10545,#10482) ;
#10510 = PRODUCT_DEFINITION('Impeller','Impeller',#10546,#10482) ;
#10511 = PRODUCT_DEFINITION('Ring','Ring',#10547,#10482) ;
#10512 = PRODUCT_DEFINITION('Motor','Motor',#10548,#10482) ;
#10513 = PRODUCT_DEFINITION('Mounting_Assembly','Mounting_Assembly',#10549,
#10482) ;
#10514 = PRODUCT_DEFINITION('Mounting_Panel','Mounting_Panel',#10550,#10482) ;
#10515 = PRODUCT_DEFINITION('Mounting_Bracket_1','Mounting_Bracket_1',#10551,
#10482) ;
#10516 = PRODUCT_DEFINITION('Mounting_Bracket_2','Mounting_Bracket_2',#10552,
#10482) ;
#10517 = PRODUCT_DEFINITION('Mounting_Bracket_3','Mounting_Bracket_3',#10553,
#10482) ;
#10518 = PRODUCT_DEFINITION('Mounting_Bracket_4','Mounting_Bracket_4',#10554,
#10482) ;
#10519 = PRODUCT_DEFINITION_FORMATION('',$,#10594) ;
#10520 = PRODUCT_DEFINITION_FORMATION('',$,#10595) ;
#10521 = PRODUCT_DEFINITION_FORMATION('',$,#10596) ;
#10522 = PRODUCT_DEFINITION_FORMATION('',$,#10597) ;
#10523 = PRODUCT_DEFINITION_FORMATION('',$,#10598) ;
#10524 = PRODUCT_DEFINITION_FORMATION('',$,#10599) ;
#10525 = PRODUCT_DEFINITION_FORMATION('',$,#10600) ;
#10526 = PRODUCT_DEFINITION_FORMATION('',$,#10601) ;
#10527 = PRODUCT_DEFINITION_FORMATION('',$,#10602) ;
#10528 = PRODUCT_DEFINITION_FORMATION('',$,#10603) ;
#10529 = PRODUCT_DEFINITION_FORMATION('',$,#10604) ;
#10530 = PRODUCT_DEFINITION_FORMATION('',$,#10605) ;
#10531 = PRODUCT_DEFINITION_FORMATION('',$,#10606) ;
#10532 = PRODUCT_DEFINITION_FORMATION('',$,#10607) ;
#10533 = PRODUCT_DEFINITION_FORMATION('',$,#10608) ;
#10534 = PRODUCT_DEFINITION_FORMATION('',$,#10609) ;
#10535 = PRODUCT_DEFINITION_FORMATION('',$,#10610) ;
#10536 = PRODUCT_DEFINITION_FORMATION('',$,#10611) ;
#10537 = PRODUCT_DEFINITION_FORMATION('',$,#10612) ;
#10538 = PRODUCT_DEFINITION_FORMATION('',$,#10613) ;
#10539 = PRODUCT_DEFINITION_FORMATION('',$,#10614) ;
#10540 = PRODUCT_DEFINITION_FORMATION('',$,#10615) ;
#10541 = PRODUCT_DEFINITION_FORMATION('',$,#10616) ;
#10542 = PRODUCT_DEFINITION_FORMATION('',$,#10617) ;
#10543 = PRODUCT_DEFINITION_FORMATION('',$,#10618) ;
#10544 = PRODUCT_DEFINITION_FORMATION('',$,#10619) ;
#10545 = PRODUCT_DEFINITION_FORMATION('',$,#10620) ;
#10546 = PRODUCT_DEFINITION_FORMATION('',$,#10621) ;
#10547 = PRODUCT_DEFINITION_FORMATION('',$,#10622) ;
#10548 = PRODUCT_DEFINITION_FORMATION('',$,#10623) ;
#10549 = PRODUCT_DEFINITION_FORMATION('',$,#10624) ;
#10550 = PRODUCT_DEFINITION_FORMATION('',$,#10625) ;
#10551 = PRODUCT_DEFINITION_FORMATION('',$,#10626) ;
#10552 = PRODUCT_DEFINITION_FORMATION('',$,#10627) ;
#10553 = PRODUCT_DEFINITION_FORMATION('',$,#10628) ;
#10554 = PRODUCT_DEFINITION_FORMATION('',$,#10629) ;
#10555 = PRODUCT_RELATED_PRODUCT_CATEGORY('MAS-638','MAS-638',(#10594)) ;
#10556 = PRODUCT_RELATED_PRODUCT_CATEGORY('Guard_Assembly',
'Guard_Assembly',(#10595)) ;
#10557 = PRODUCT_RELATED_PRODUCT_CATEGORY('Guard_Mounting_Ring_1',
'Guard_Mounting_Ring_1',(#10596)) ;
#10558 = PRODUCT_RELATED_PRODUCT_CATEGORY('Guard_Mounting_Ring_2',
'Guard_Mounting_Ring_2',(#10597)) ;
#10559 = PRODUCT_RELATED_PRODUCT_CATEGORY('Guard_Ring_1','Guard_Ring_1',(#10598)) ;
#10560 = PRODUCT_RELATED_PRODUCT_CATEGORY('Guard_Ring_2','Guard_Ring_2',(#10599)) ;
#10561 = PRODUCT_RELATED_PRODUCT_CATEGORY('Guard_Ring_3','Guard_Ring_3',(#10600)) ;
#10562 = PRODUCT_RELATED_PRODUCT_CATEGORY('Guard_Ring_4','Guard_Ring_4',(#10601)) ;
#10563 = PRODUCT_RELATED_PRODUCT_CATEGORY('Guard_Ring_5','Guard_Ring_5',(#10602)) ;
#10564 = PRODUCT_RELATED_PRODUCT_CATEGORY('Guard_Ring_6','Guard_Ring_6',(#10603)) ;
#10565 = PRODUCT_RELATED_PRODUCT_CATEGORY('Guard_Ring_7','Guard_Ring_7',(#10604)) ;
#10566 = PRODUCT_RELATED_PRODUCT_CATEGORY('Guard_Ring_8','Guard_Ring_8',(#10605)) ;
#10567 = PRODUCT_RELATED_PRODUCT_CATEGORY('Guard_Ring_9','Guard_Ring_9',(#10606)) ;
#10568 = PRODUCT_RELATED_PRODUCT_CATEGORY('Guard_Ring_10','Guard_Ring_10',
(#10607)) ;
#10569 = PRODUCT_RELATED_PRODUCT_CATEGORY('Guard_Ring_11','Guard_Ring_11',
(#10608)) ;
#10570 = PRODUCT_RELATED_PRODUCT_CATEGORY('Guard_Ring_12','Guard_Ring_12',
(#10609)) ;
#10571 = PRODUCT_RELATED_PRODUCT_CATEGORY('Guard_Ring_13','Guard_Ring_13',
(#10610)) ;
#10572 = PRODUCT_RELATED_PRODUCT_CATEGORY('Guard_Ring_14','Guard_Ring_14',
(#10611)) ;
#10573 = PRODUCT_RELATED_PRODUCT_CATEGORY('Guard_Ring_15','Guard_Ring_15',
(#10612)) ;
#10574 = PRODUCT_RELATED_PRODUCT_CATEGORY('Guard_Ring_16','Guard_Ring_16',
(#10613)) ;
#10575 = PRODUCT_RELATED_PRODUCT_CATEGORY('Guard_Ring_17','Guard_Ring_17',
(#10614)) ;
#10576 = PRODUCT_RELATED_PRODUCT_CATEGORY('Guard_Ring_18','Guard_Ring_18',
(#10615)) ;
#10577 = PRODUCT_RELATED_PRODUCT_CATEGORY('Guard_Ring_19','Guard_Ring_19',
(#10616)) ;
#10578 = PRODUCT_RELATED_PRODUCT_CATEGORY('Guard_Ring_20','Guard_Ring_20',
(#10617)) ;
#10579 = PRODUCT_RELATED_PRODUCT_CATEGORY('Guard_Ring_21','Guard_Ring_21',
(#10618)) ;
#10580 = PRODUCT_RELATED_PRODUCT_CATEGORY('Guard_Ring_22','Guard_Ring_22',
(#10619)) ;
#10581 = PRODUCT_RELATED_PRODUCT_CATEGORY('Fan_Assembly','Fan_Assembly',(#10620)) ;
#10582 = PRODUCT_RELATED_PRODUCT_CATEGORY('Impeller','Impeller',(#10621)) ;
#10583 = PRODUCT_RELATED_PRODUCT_CATEGORY('Ring','Ring',(#10622)) ;
#10584 = PRODUCT_RELATED_PRODUCT_CATEGORY('Motor','Motor',(#10623)) ;
#10585 = PRODUCT_RELATED_PRODUCT_CATEGORY('Mounting_Assembly',
'Mounting_Assembly',(#10624)) ;
#10586 = PRODUCT_RELATED_PRODUCT_CATEGORY('Mounting_Panel',
'Mounting_Panel',(#10625)) ;
#10587 = PRODUCT_RELATED_PRODUCT_CATEGORY('Mounting_Bracket_1',
'Mounting_Bracket_1',(#10626)) ;
#10588 = PRODUCT_RELATED_PRODUCT_CATEGORY('Mounting_Bracket_2',
'Mounting_Bracket_2',(#10627)) ;
#10589 = PRODUCT_RELATED_PRODUCT_CATEGORY('Mounting_Bracket_3',
'Mounting_Bracket_3',(#10628)) ;
#10590 = PRODUCT_RELATED_PRODUCT_CATEGORY('Mounting_Bracket_4',
'Mounting_Bracket_4',(#10629)) ;
#10591 = APPLICATION_PROTOCOL_DEFINITION('international standard',
'automotive_design',2009,#10592) ;
#10592 = APPLICATION_CONTEXT(
'Core Data for Automotive Mechanical Design Process') ;
#10593 = PRODUCT_CONTEXT('part definition',#10592,'mechanical') ;
#10594 = PRODUCT('MAS-638','MAS-638',$,(#10593)) ;
#10595 = PRODUCT('Guard_Assembly','Guard_Assembly',$,(#10593)) ;
#10596 = PRODUCT('Guard_Mounting_Ring_1','Guard_Mounting_Ring_1',$,(#10593)) ;
#10597 = PRODUCT('Guard_Mounting_Ring_2','Guard_Mounting_Ring_2',$,(#10593)) ;
#10598 = PRODUCT('Guard_Ring_1','Guard_Ring_1',$,(#10593)) ;
#10599 = PRODUCT('Guard_Ring_2','Guard_Ring_2',$,(#10593)) ;
#10600 = PRODUCT('Guard_Ring_3','Guard_Ring_3',$,(#10593)) ;
#10601 = PRODUCT('Guard_Ring_4','Guard_Ring_4',$,(#10593)) ;
#10602 = PRODUCT('Guard_Ring_5','Guard_Ring_5',$,(#10593)) ;
#10603 = PRODUCT('Guard_Ring_6','Guard_Ring_6',$,(#10593)) ;
#10604 = PRODUCT('Guard_Ring_7','Guard_Ring_7',$,(#10593)) ;
#10605 = PRODUCT('Guard_Ring_8','Guard_Ring_8',$,(#10593)) ;
#10606 = PRODUCT('Guard_Ring_9','Guard_Ring_9',$,(#10593)) ;
#10607 = PRODUCT('Guard_Ring_10','Guard_Ring_10',$,(#10593)) ;
#10608 = PRODUCT('Guard_Ring_11','Guard_Ring_11',$,(#10593)) ;
#10609 = PRODUCT('Guard_Ring_12','Guard_Ring_12',$,(#10593)) ;
#10610 = PRODUCT('Guard_Ring_13','Guard_Ring_13',$,(#10593)) ;
#10611 = PRODUCT('Guard_Ring_14','Guard_Ring_14',$,(#10593)) ;
#10612 = PRODUCT('Guard_Ring_15','Guard_Ring_15',$,(#10593)) ;
#10613 = PRODUCT('Guard_Ring_16','Guard_Ring_16',$,(#10593)) ;
#10614 = PRODUCT('Guard_Ring_17','Guard_Ring_17',$,(#10593)) ;
#10615 = PRODUCT('Guard_Ring_18','Guard_Ring_18',$,(#10593)) ;
#10616 = PRODUCT('Guard_Ring_19','Guard_Ring_19',$,(#10593)) ;
#10617 = PRODUCT('Guard_Ring_20','Guard_Ring_20',$,(#10593)) ;
#10618 = PRODUCT('Guard_Ring_21','Guard_Ring_21',$,(#10593)) ;
#10619 = PRODUCT('Guard_Ring_22','Guard_Ring_22',$,(#10593)) ;
#10620 = PRODUCT('Fan_Assembly','Fan_Assembly',$,(#10593)) ;
#10621 = PRODUCT('Impeller','Impeller',$,(#10593)) ;
#10622 = PRODUCT('Ring','Ring',$,(#10593)) ;
#10623 = PRODUCT('Motor','Motor',$,(#10593)) ;
#10624 = PRODUCT('Mounting_Assembly','Mounting_Assembly',$,(#10593)) ;
#10625 = PRODUCT('Mounting_Panel','Mounting_Panel',$,(#10593)) ;
#10626 = PRODUCT('Mounting_Bracket_1','Mounting_Bracket_1',$,(#10593)) ;
#10627 = PRODUCT('Mounting_Bracket_2','Mounting_Bracket_2',$,(#10593)) ;
#10628 = PRODUCT('Mounting_Bracket_3','Mounting_Bracket_3',$,(#10593)) ;
#10629 = PRODUCT('Mounting_Bracket_4','Mounting_Bracket_4',$,(#10593)) ;
#10630 = PRESENTATION_STYLE_ASSIGNMENT((#10634)) ;
#10631 = PRESENTATION_STYLE_ASSIGNMENT((#10635)) ;
#10632 = PRESENTATION_STYLE_ASSIGNMENT((#10636)) ;
#10633 = PRESENTATION_STYLE_ASSIGNMENT((#10637)) ;
#10634 = SURFACE_STYLE_USAGE(.BOTH.,#10638) ;
#10635 = SURFACE_STYLE_USAGE(.BOTH.,#10639) ;
#10636 = SURFACE_STYLE_USAGE(.BOTH.,#10640) ;
#10637 = SURFACE_STYLE_USAGE(.BOTH.,#10641) ;
#10638 = SURFACE_SIDE_STYLE('',(#10642)) ;
#10639 = SURFACE_SIDE_STYLE('',(#10643)) ;
#10640 = SURFACE_SIDE_STYLE('',(#10644)) ;
#10641 = SURFACE_SIDE_STYLE('',(#10645)) ;
#10642 = SURFACE_STYLE_FILL_AREA(#10646) ;
#10643 = SURFACE_STYLE_FILL_AREA(#10647) ;
#10644 = SURFACE_STYLE_FILL_AREA(#10648) ;
#10645 = SURFACE_STYLE_FILL_AREA(#10649) ;
#10646 = FILL_AREA_STYLE('Steel - Satin',(#10650)) ;
#10647 = FILL_AREA_STYLE('Opaque(25,25,25)',(#10651)) ;
#10648 = FILL_AREA_STYLE('Opaque(202,209,238)',(#10652)) ;
#10649 = FILL_AREA_STYLE('Opaque(232,173,35)',(#10653)) ;
#10650 = FILL_AREA_STYLE_COLOUR('Steel - Satin',#10654) ;
#10651 = FILL_AREA_STYLE_COLOUR('Opaque(25,25,25)',#10655) ;
#10652 = FILL_AREA_STYLE_COLOUR('Opaque(202,209,238)',#10656) ;
#10653 = FILL_AREA_STYLE_COLOUR('Opaque(232,173,35)',#10657) ;
#10654 = COLOUR_RGB('Steel - Satin', 0.09019608, 0.27058824, 0.51372549) ;
#10655 = COLOUR_RGB('Opaque(25,25,25)', 0.09019608, 0.27058824, 0.51372549) ;
#10656 = COLOUR_RGB('Opaque(202,209,238)', 0.40784314, 0.44705882, 0.49803922) ;
#10657 = COLOUR_RGB('Opaque(232,173,35)', 0.09019608, 0.27058824, 0.51372549) ;
ENDSEC;
END-ISO-10303-21;
